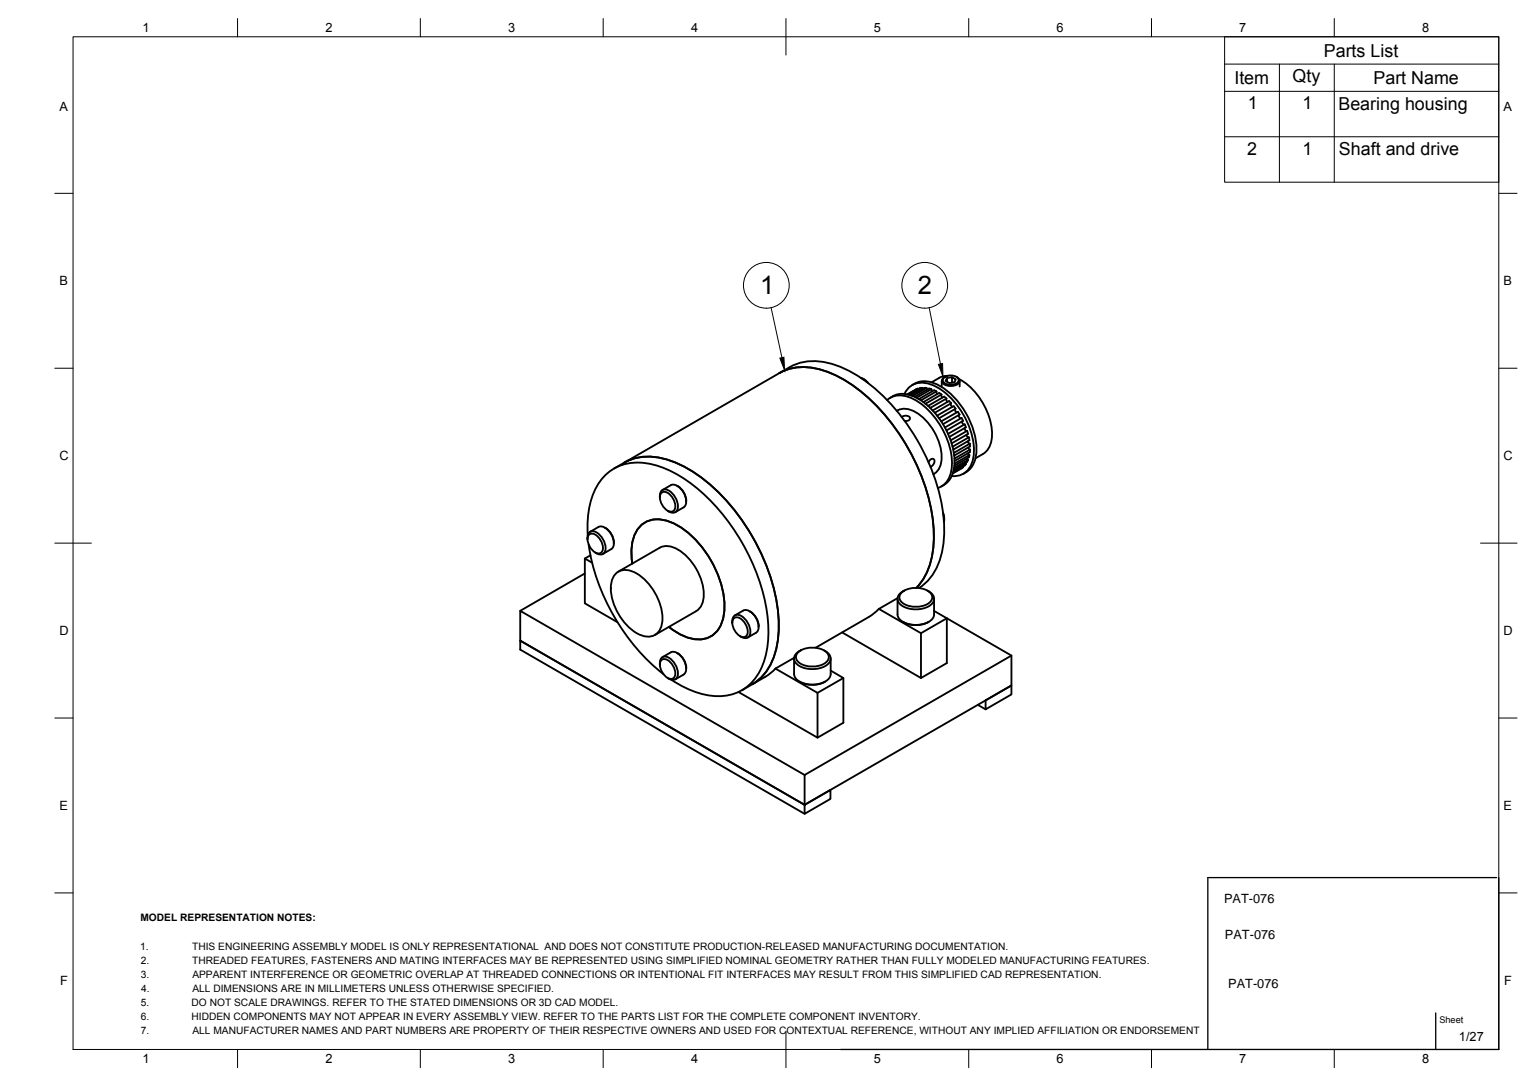
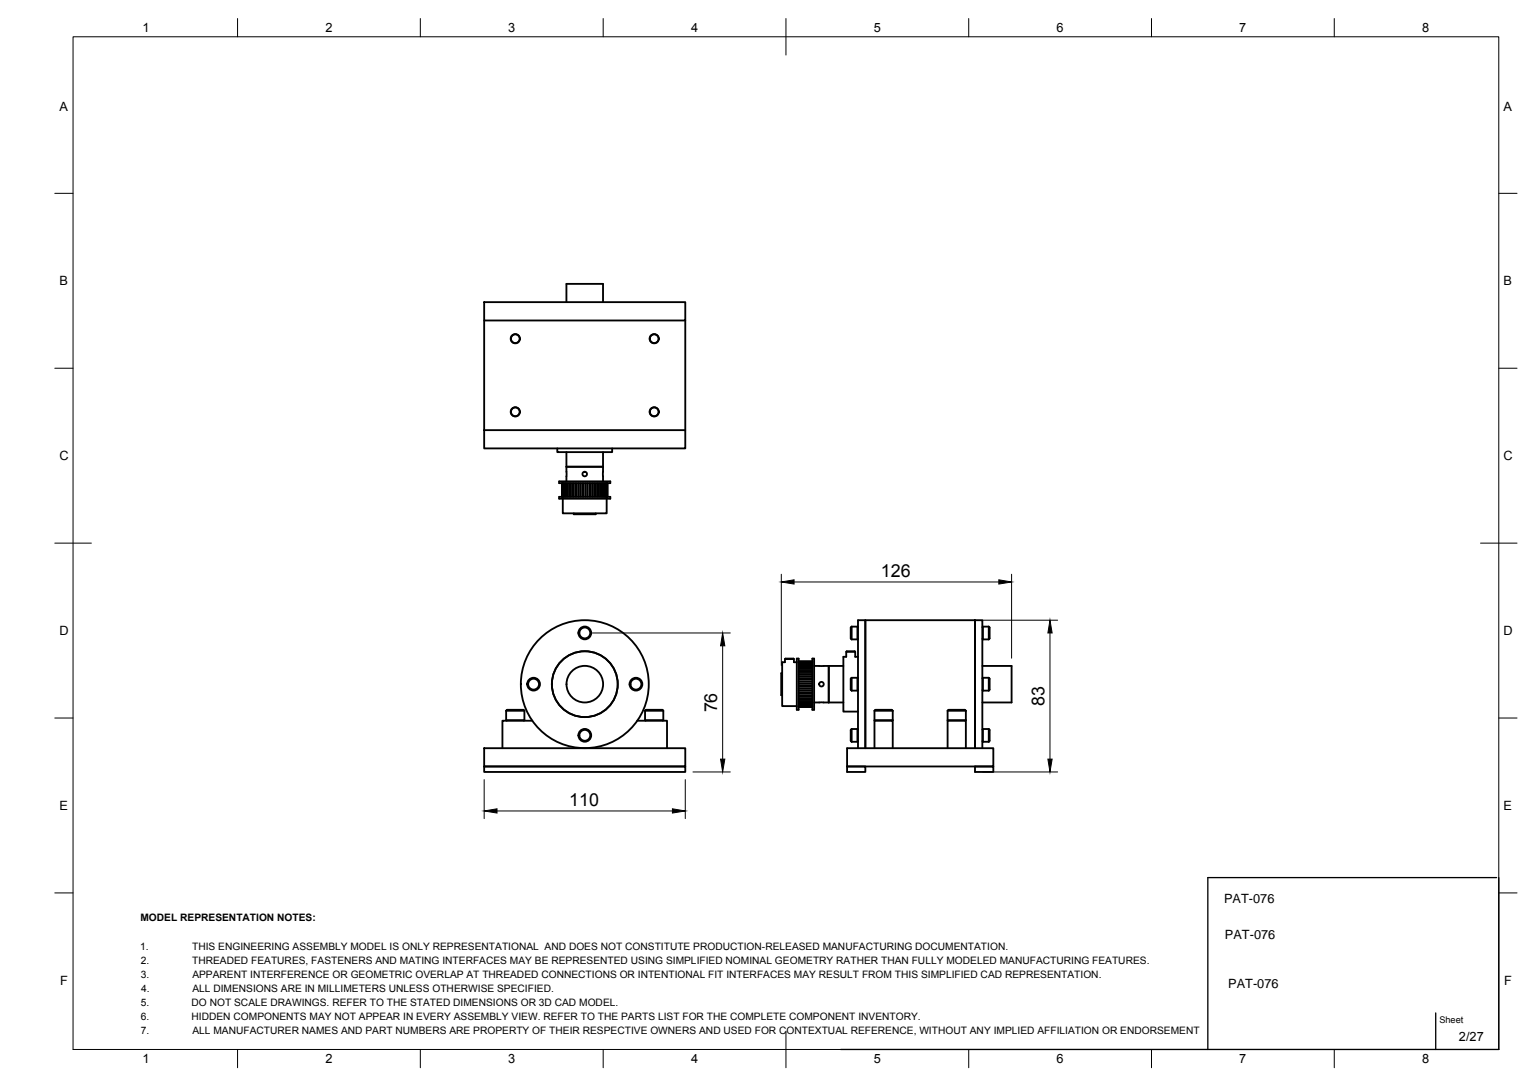
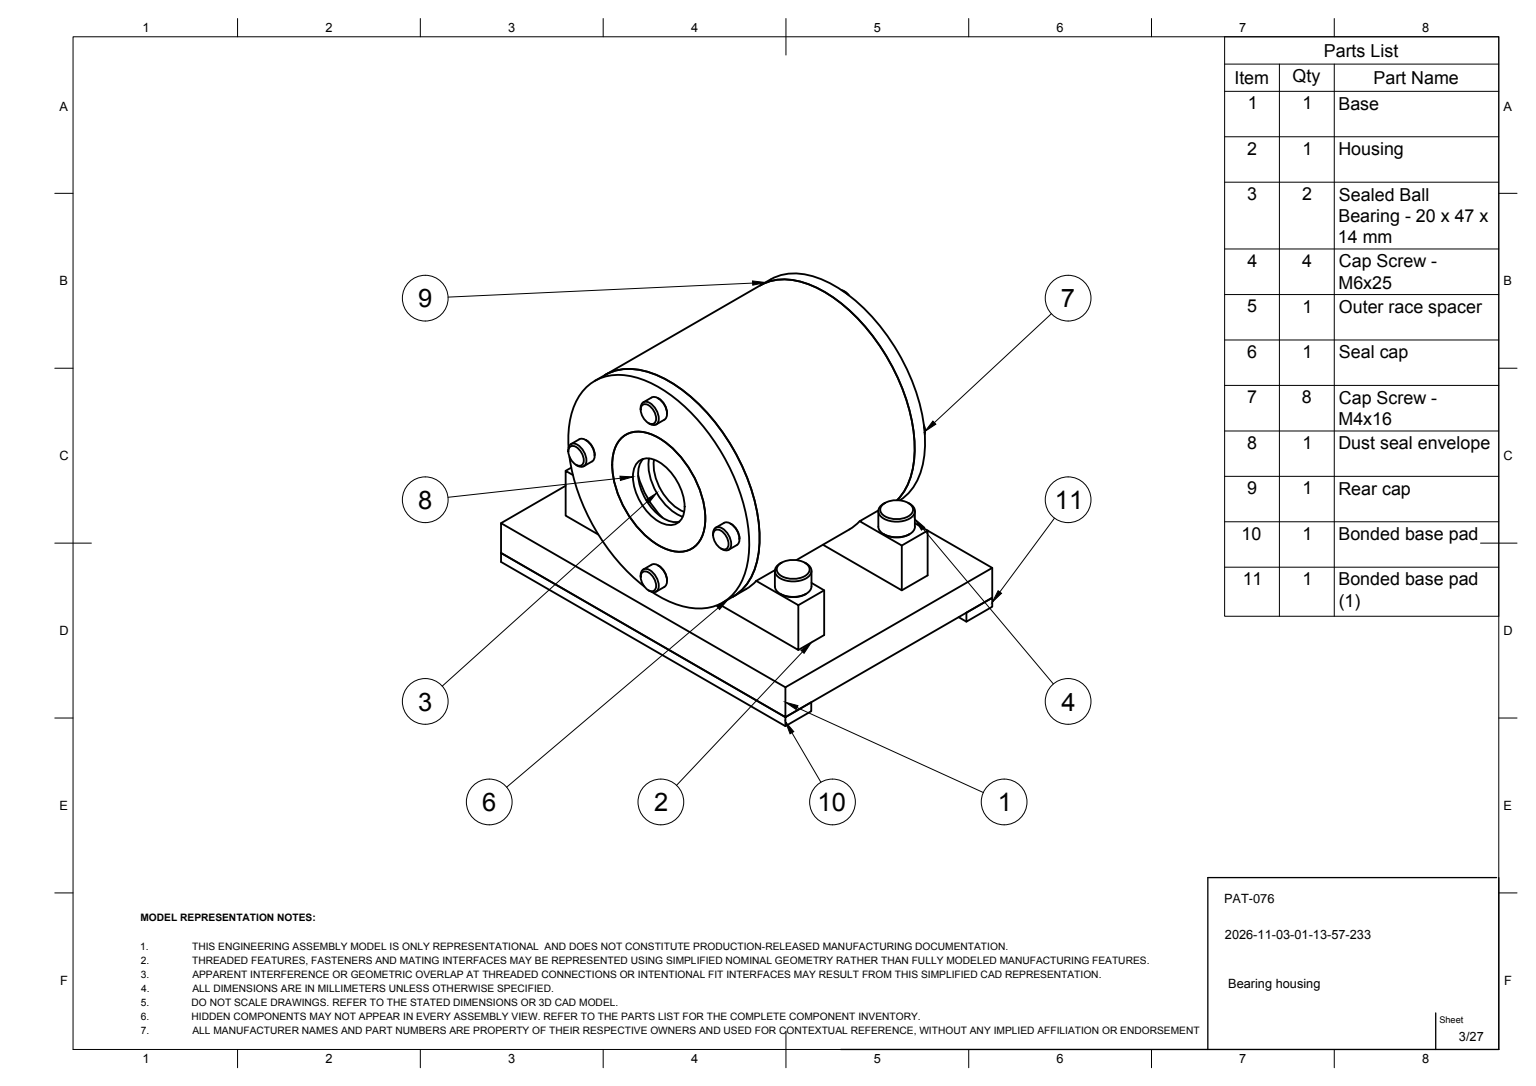
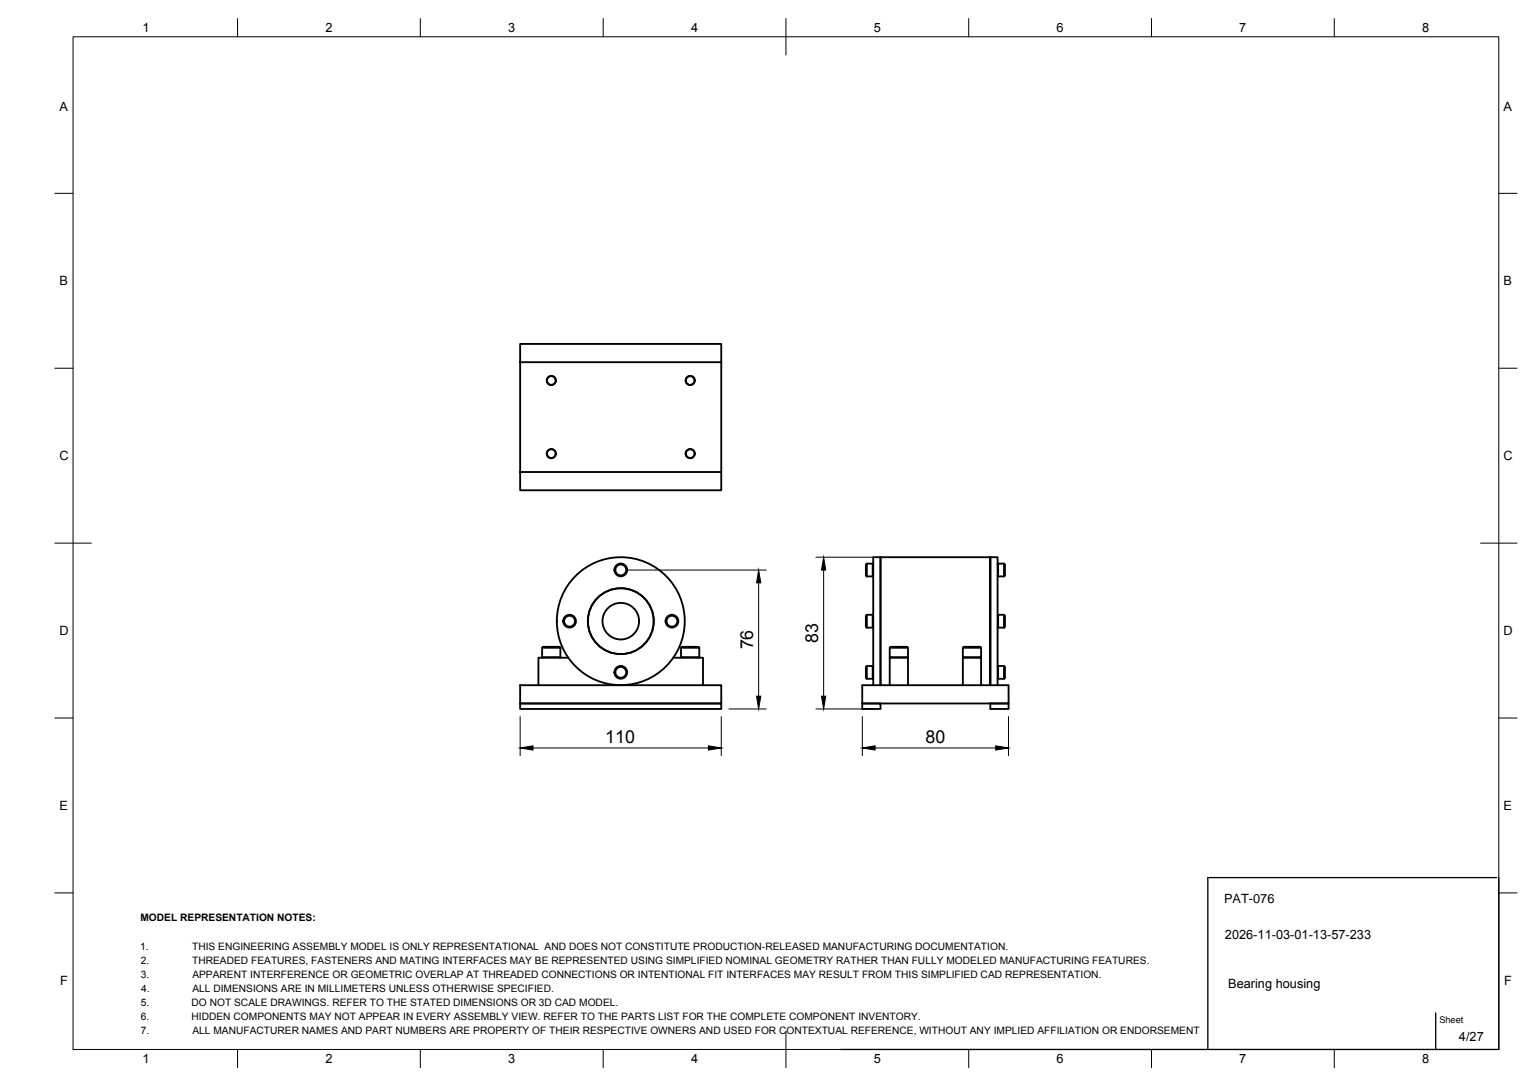
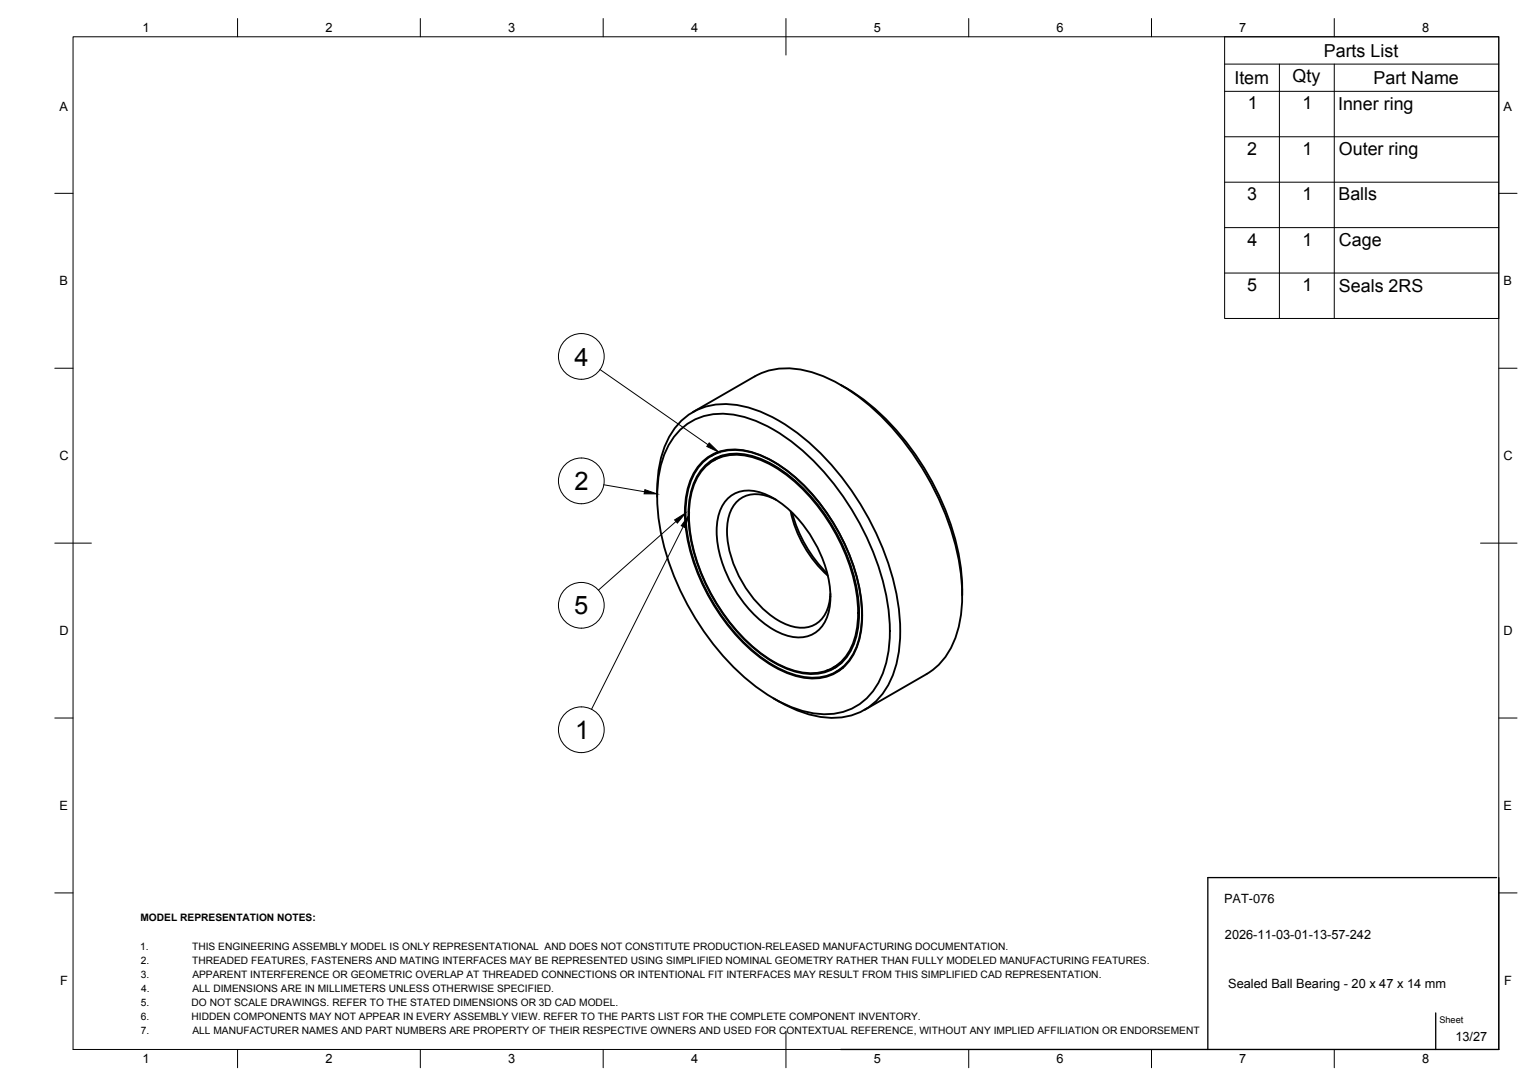
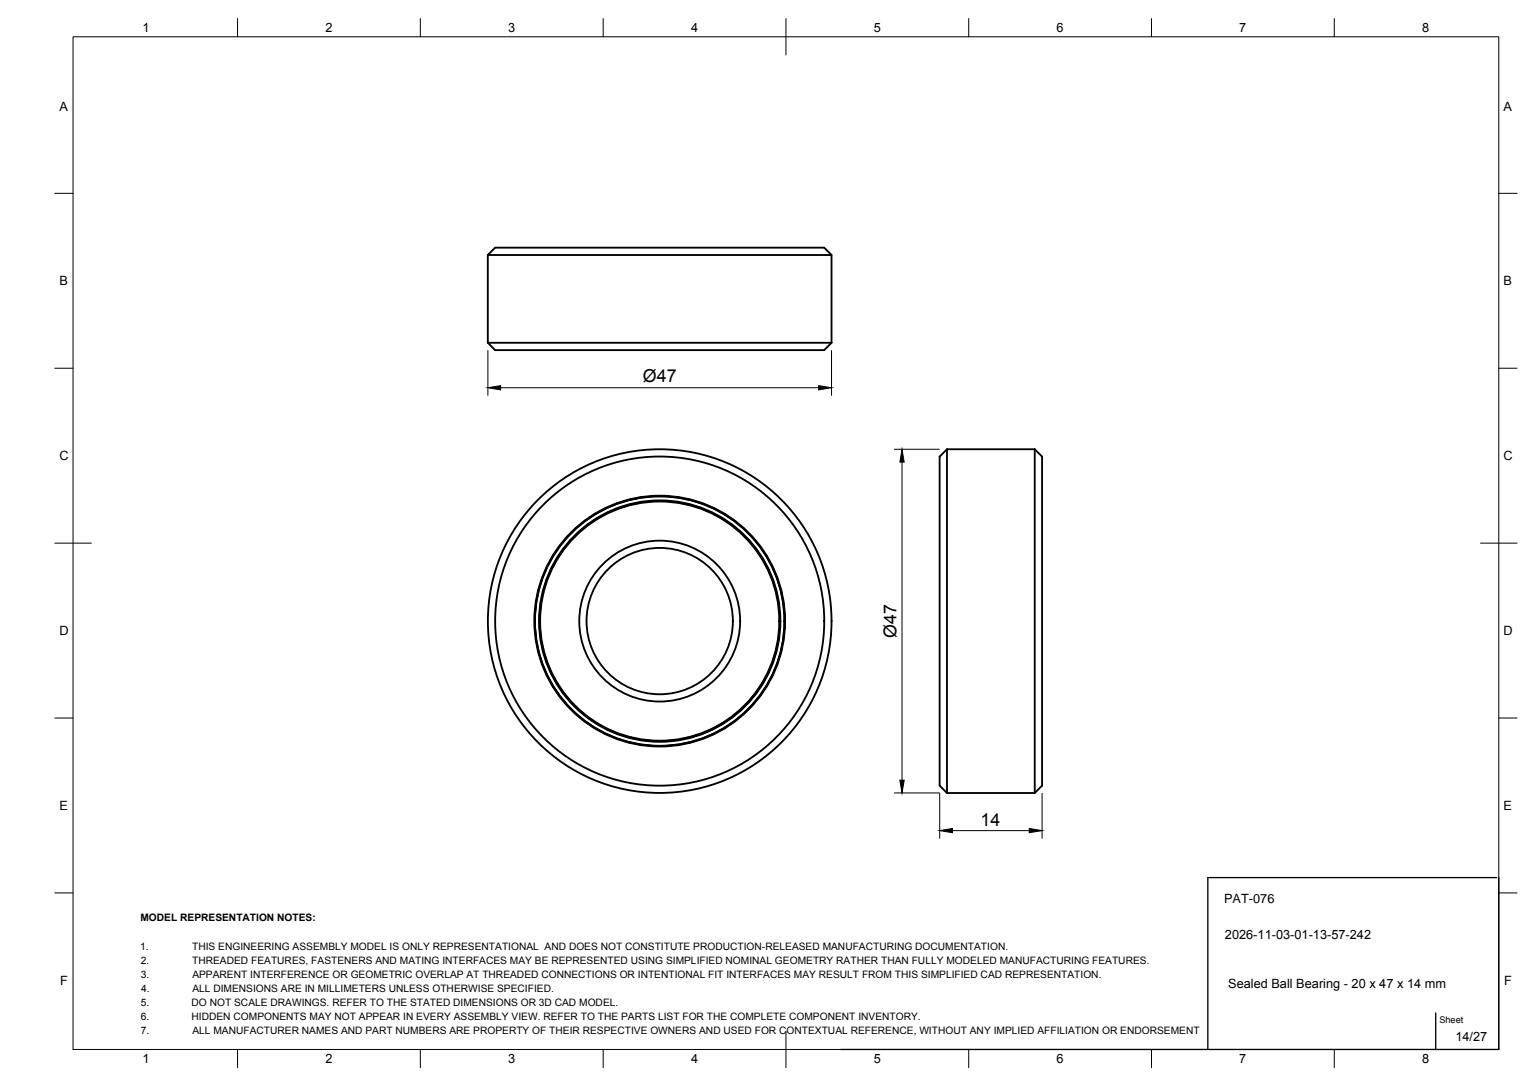
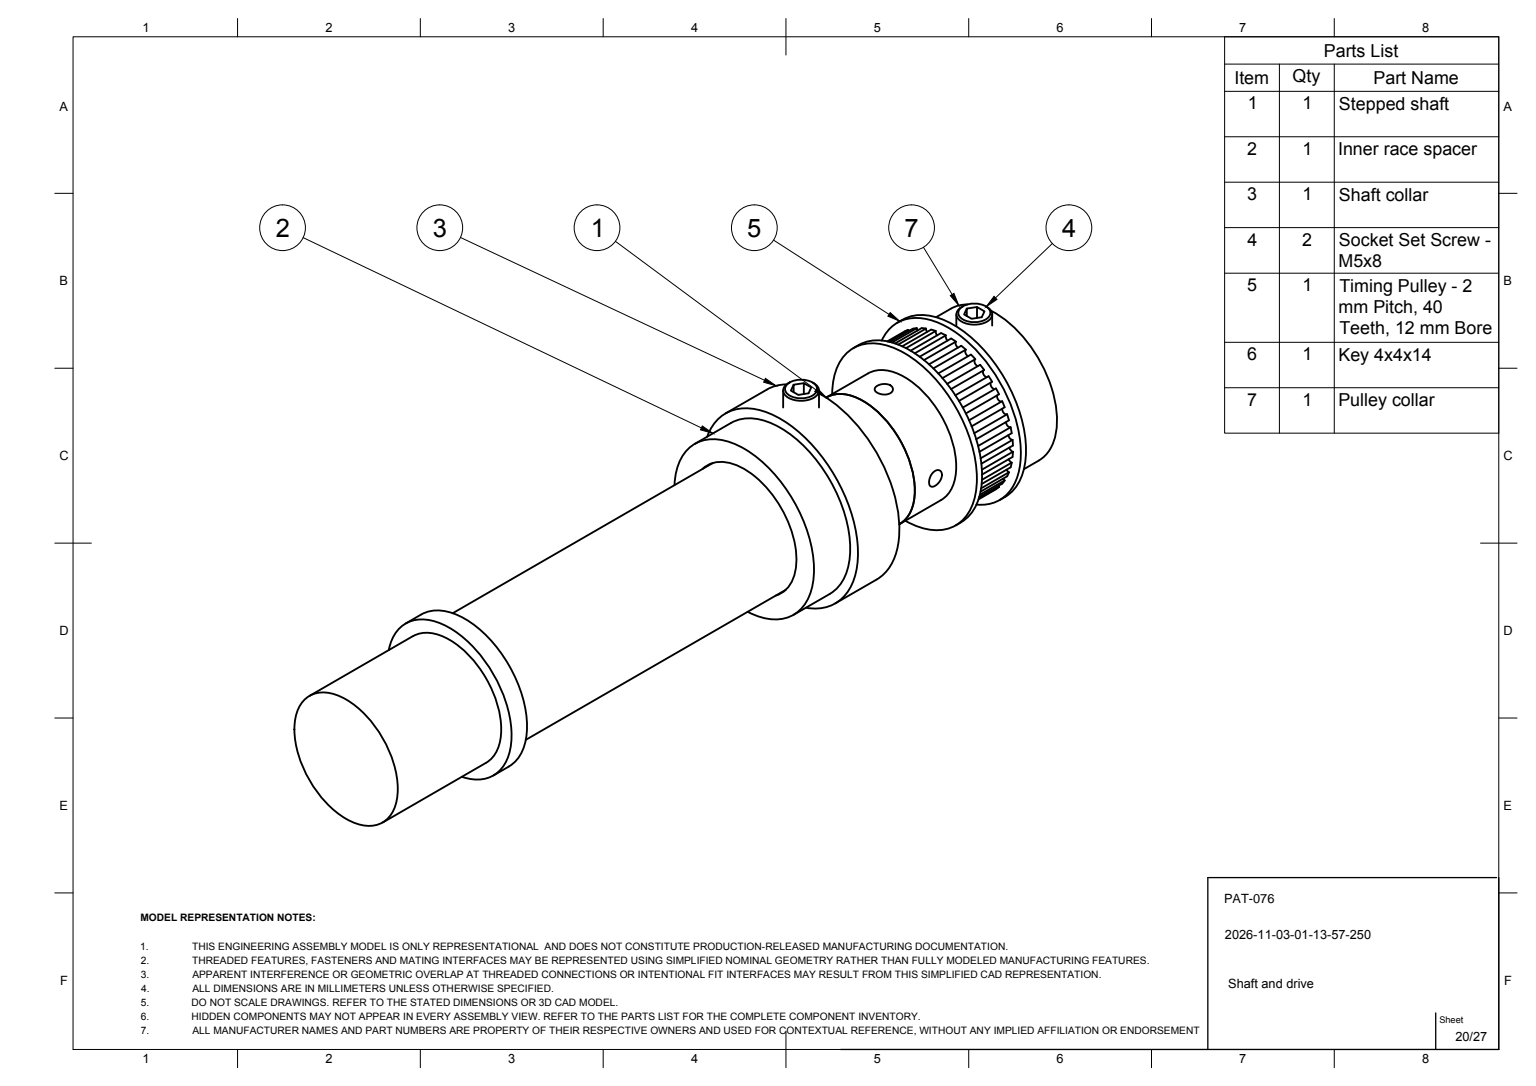
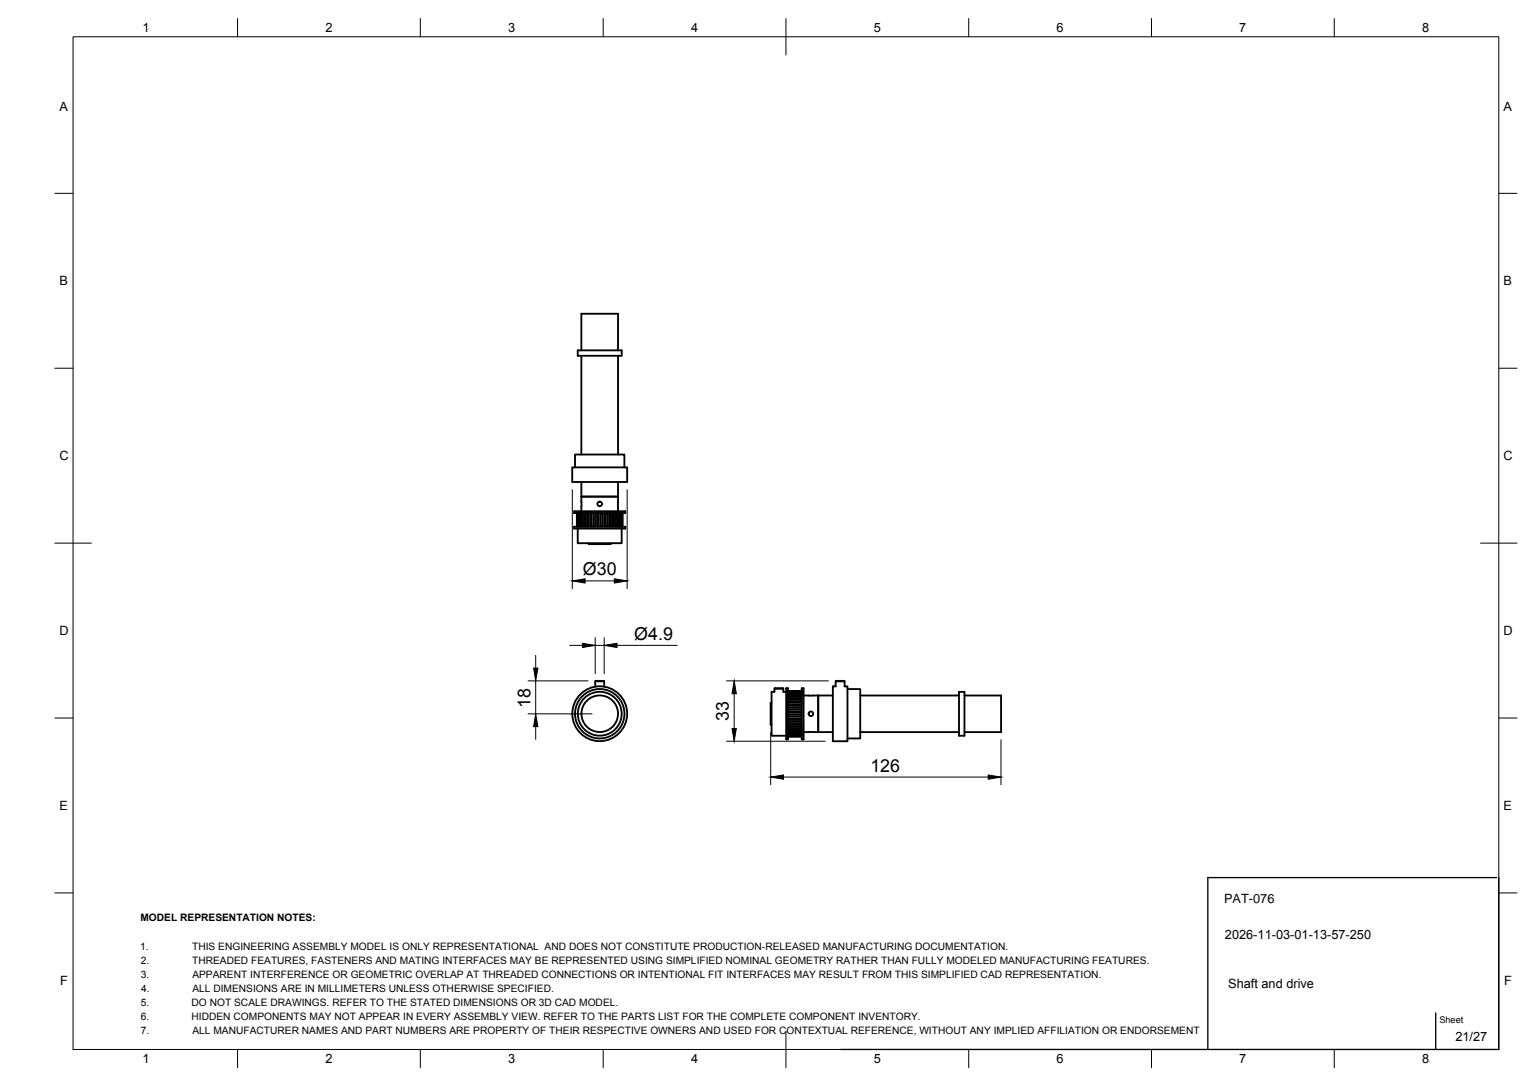
ISO-10303-21;
HEADER;
/* Generated by software containing ST-Developer
 * from STEP Tools, Inc. (www.steptools.com) 
 */

FILE_DESCRIPTION(
/* description */ ('Overhung pulley bearing cartridge'),
/* implementation_level */ '2;1');

FILE_NAME(
/* name */ 'PAT-076',
/* time_stamp */ '2026-10-28T03:22:33-07:00',
/* author */ (''),
/* organization */ (''),
/* preprocessor_version */ 'ST-DEVELOPER v20.2',
/* originating_system */ 'Autodesk Translation Framework v15.17.0.0',
/* authorisation */ '');

FILE_SCHEMA (('AUTOMOTIVE_DESIGN { 1 0 10303 214 3 1 1 }'));
ENDSEC;

DATA;
#10=MECHANICAL_DESIGN_GEOMETRIC_PRESENTATION_REPRESENTATION('',(#283,#284,
#285,#286,#287,#288,#289,#290,#291,#292,#293,#294,#295,#296,#297,#298,#299,
#300,#301,#302,#303,#304,#305,#306,#307,#308,#309,#310,#311,#312),#10963);
#11=ORIENTED_CLOSED_SHELL('',*,#5672,.F.);
#12=ORIENTED_CLOSED_SHELL('',*,#5674,.F.);
#13=BREP_WITH_VOIDS('Body1',#5671,(#11));
#14=BREP_WITH_VOIDS('Body1',#5673,(#12));
#15=ITEM_DEFINED_TRANSFORMATION($,$,#6112,#6240);
#16=ITEM_DEFINED_TRANSFORMATION($,$,#6132,#6241);
#17=ITEM_DEFINED_TRANSFORMATION($,$,#6152,#6242);
#18=ITEM_DEFINED_TRANSFORMATION($,$,#6169,#6243);
#19=ITEM_DEFINED_TRANSFORMATION($,$,#6223,#6244);
#20=ITEM_DEFINED_TRANSFORMATION($,$,#5927,#6297);
#21=ITEM_DEFINED_TRANSFORMATION($,$,#5946,#6298);
#22=ITEM_DEFINED_TRANSFORMATION($,$,#6025,#6299);
#23=ITEM_DEFINED_TRANSFORMATION($,$,#6034,#6300);
#24=ITEM_DEFINED_TRANSFORMATION($,$,#6063,#6301);
#25=ITEM_DEFINED_TRANSFORMATION($,$,#6072,#6302);
#26=ITEM_DEFINED_TRANSFORMATION($,$,#6097,#6303);
#27=ITEM_DEFINED_TRANSFORMATION($,$,#6104,#6304);
#28=ITEM_DEFINED_TRANSFORMATION($,$,#6111,#6305);
#29=ITEM_DEFINED_TRANSFORMATION($,$,#6245,#6306);
#30=ITEM_DEFINED_TRANSFORMATION($,$,#6245,#6307);
#31=ITEM_DEFINED_TRANSFORMATION($,$,#6111,#6308);
#32=ITEM_DEFINED_TRANSFORMATION($,$,#6245,#6309);
#33=ITEM_DEFINED_TRANSFORMATION($,$,#6245,#6310);
#34=ITEM_DEFINED_TRANSFORMATION($,$,#6271,#6311);
#35=ITEM_DEFINED_TRANSFORMATION($,$,#6271,#6312);
#36=ITEM_DEFINED_TRANSFORMATION($,$,#6271,#6313);
#37=ITEM_DEFINED_TRANSFORMATION($,$,#6271,#6314);
#38=ITEM_DEFINED_TRANSFORMATION($,$,#6271,#6315);
#39=ITEM_DEFINED_TRANSFORMATION($,$,#6271,#6316);
#40=ITEM_DEFINED_TRANSFORMATION($,$,#6271,#6317);
#41=ITEM_DEFINED_TRANSFORMATION($,$,#6271,#6318);
#42=ITEM_DEFINED_TRANSFORMATION($,$,#6320,#6678);
#43=ITEM_DEFINED_TRANSFORMATION($,$,#6345,#6679);
#44=ITEM_DEFINED_TRANSFORMATION($,$,#6354,#6680);
#45=ITEM_DEFINED_TRANSFORMATION($,$,#6369,#6681);
#46=ITEM_DEFINED_TRANSFORMATION($,$,#6661,#6682);
#47=ITEM_DEFINED_TRANSFORMATION($,$,#6384,#6683);
#48=ITEM_DEFINED_TRANSFORMATION($,$,#6650,#6684);
#49=ITEM_DEFINED_TRANSFORMATION($,$,#6661,#6685);
#50=ITEM_DEFINED_TRANSFORMATION($,$,#5926,#6686);
#51=ITEM_DEFINED_TRANSFORMATION($,$,#6319,#6687);
#52=(
REPRESENTATION_RELATIONSHIP($,$,#11068,#11067)
REPRESENTATION_RELATIONSHIP_WITH_TRANSFORMATION(#15)
SHAPE_REPRESENTATION_RELATIONSHIP()
);
#53=(
REPRESENTATION_RELATIONSHIP($,$,#11069,#11067)
REPRESENTATION_RELATIONSHIP_WITH_TRANSFORMATION(#16)
SHAPE_REPRESENTATION_RELATIONSHIP()
);
#54=(
REPRESENTATION_RELATIONSHIP($,$,#11070,#11067)
REPRESENTATION_RELATIONSHIP_WITH_TRANSFORMATION(#17)
SHAPE_REPRESENTATION_RELATIONSHIP()
);
#55=(
REPRESENTATION_RELATIONSHIP($,$,#11071,#11067)
REPRESENTATION_RELATIONSHIP_WITH_TRANSFORMATION(#18)
SHAPE_REPRESENTATION_RELATIONSHIP()
);
#56=(
REPRESENTATION_RELATIONSHIP($,$,#11072,#11067)
REPRESENTATION_RELATIONSHIP_WITH_TRANSFORMATION(#19)
SHAPE_REPRESENTATION_RELATIONSHIP()
);
#57=(
REPRESENTATION_RELATIONSHIP($,$,#11059,#11058)
REPRESENTATION_RELATIONSHIP_WITH_TRANSFORMATION(#20)
SHAPE_REPRESENTATION_RELATIONSHIP()
);
#58=(
REPRESENTATION_RELATIONSHIP($,$,#11060,#11058)
REPRESENTATION_RELATIONSHIP_WITH_TRANSFORMATION(#21)
SHAPE_REPRESENTATION_RELATIONSHIP()
);
#59=(
REPRESENTATION_RELATIONSHIP($,$,#11061,#11058)
REPRESENTATION_RELATIONSHIP_WITH_TRANSFORMATION(#22)
SHAPE_REPRESENTATION_RELATIONSHIP()
);
#60=(
REPRESENTATION_RELATIONSHIP($,$,#11062,#11058)
REPRESENTATION_RELATIONSHIP_WITH_TRANSFORMATION(#23)
SHAPE_REPRESENTATION_RELATIONSHIP()
);
#61=(
REPRESENTATION_RELATIONSHIP($,$,#11063,#11058)
REPRESENTATION_RELATIONSHIP_WITH_TRANSFORMATION(#24)
SHAPE_REPRESENTATION_RELATIONSHIP()
);
#62=(
REPRESENTATION_RELATIONSHIP($,$,#11064,#11058)
REPRESENTATION_RELATIONSHIP_WITH_TRANSFORMATION(#25)
SHAPE_REPRESENTATION_RELATIONSHIP()
);
#63=(
REPRESENTATION_RELATIONSHIP($,$,#11065,#11058)
REPRESENTATION_RELATIONSHIP_WITH_TRANSFORMATION(#26)
SHAPE_REPRESENTATION_RELATIONSHIP()
);
#64=(
REPRESENTATION_RELATIONSHIP($,$,#11066,#11058)
REPRESENTATION_RELATIONSHIP_WITH_TRANSFORMATION(#27)
SHAPE_REPRESENTATION_RELATIONSHIP()
);
#65=(
REPRESENTATION_RELATIONSHIP($,$,#11067,#11058)
REPRESENTATION_RELATIONSHIP_WITH_TRANSFORMATION(#28)
SHAPE_REPRESENTATION_RELATIONSHIP()
);
#66=(
REPRESENTATION_RELATIONSHIP($,$,#11073,#11058)
REPRESENTATION_RELATIONSHIP_WITH_TRANSFORMATION(#29)
SHAPE_REPRESENTATION_RELATIONSHIP()
);
#67=(
REPRESENTATION_RELATIONSHIP($,$,#11073,#11058)
REPRESENTATION_RELATIONSHIP_WITH_TRANSFORMATION(#30)
SHAPE_REPRESENTATION_RELATIONSHIP()
);
#68=(
REPRESENTATION_RELATIONSHIP($,$,#11067,#11058)
REPRESENTATION_RELATIONSHIP_WITH_TRANSFORMATION(#31)
SHAPE_REPRESENTATION_RELATIONSHIP()
);
#69=(
REPRESENTATION_RELATIONSHIP($,$,#11073,#11058)
REPRESENTATION_RELATIONSHIP_WITH_TRANSFORMATION(#32)
SHAPE_REPRESENTATION_RELATIONSHIP()
);
#70=(
REPRESENTATION_RELATIONSHIP($,$,#11073,#11058)
REPRESENTATION_RELATIONSHIP_WITH_TRANSFORMATION(#33)
SHAPE_REPRESENTATION_RELATIONSHIP()
);
#71=(
REPRESENTATION_RELATIONSHIP($,$,#11074,#11058)
REPRESENTATION_RELATIONSHIP_WITH_TRANSFORMATION(#34)
SHAPE_REPRESENTATION_RELATIONSHIP()
);
#72=(
REPRESENTATION_RELATIONSHIP($,$,#11074,#11058)
REPRESENTATION_RELATIONSHIP_WITH_TRANSFORMATION(#35)
SHAPE_REPRESENTATION_RELATIONSHIP()
);
#73=(
REPRESENTATION_RELATIONSHIP($,$,#11074,#11058)
REPRESENTATION_RELATIONSHIP_WITH_TRANSFORMATION(#36)
SHAPE_REPRESENTATION_RELATIONSHIP()
);
#74=(
REPRESENTATION_RELATIONSHIP($,$,#11074,#11058)
REPRESENTATION_RELATIONSHIP_WITH_TRANSFORMATION(#37)
SHAPE_REPRESENTATION_RELATIONSHIP()
);
#75=(
REPRESENTATION_RELATIONSHIP($,$,#11074,#11058)
REPRESENTATION_RELATIONSHIP_WITH_TRANSFORMATION(#38)
SHAPE_REPRESENTATION_RELATIONSHIP()
);
#76=(
REPRESENTATION_RELATIONSHIP($,$,#11074,#11058)
REPRESENTATION_RELATIONSHIP_WITH_TRANSFORMATION(#39)
SHAPE_REPRESENTATION_RELATIONSHIP()
);
#77=(
REPRESENTATION_RELATIONSHIP($,$,#11074,#11058)
REPRESENTATION_RELATIONSHIP_WITH_TRANSFORMATION(#40)
SHAPE_REPRESENTATION_RELATIONSHIP()
);
#78=(
REPRESENTATION_RELATIONSHIP($,$,#11074,#11058)
REPRESENTATION_RELATIONSHIP_WITH_TRANSFORMATION(#41)
SHAPE_REPRESENTATION_RELATIONSHIP()
);
#79=(
REPRESENTATION_RELATIONSHIP($,$,#11076,#11075)
REPRESENTATION_RELATIONSHIP_WITH_TRANSFORMATION(#42)
SHAPE_REPRESENTATION_RELATIONSHIP()
);
#80=(
REPRESENTATION_RELATIONSHIP($,$,#11077,#11075)
REPRESENTATION_RELATIONSHIP_WITH_TRANSFORMATION(#43)
SHAPE_REPRESENTATION_RELATIONSHIP()
);
#81=(
REPRESENTATION_RELATIONSHIP($,$,#11078,#11075)
REPRESENTATION_RELATIONSHIP_WITH_TRANSFORMATION(#44)
SHAPE_REPRESENTATION_RELATIONSHIP()
);
#82=(
REPRESENTATION_RELATIONSHIP($,$,#11079,#11075)
REPRESENTATION_RELATIONSHIP_WITH_TRANSFORMATION(#45)
SHAPE_REPRESENTATION_RELATIONSHIP()
);
#83=(
REPRESENTATION_RELATIONSHIP($,$,#11082,#11075)
REPRESENTATION_RELATIONSHIP_WITH_TRANSFORMATION(#46)
SHAPE_REPRESENTATION_RELATIONSHIP()
);
#84=(
REPRESENTATION_RELATIONSHIP($,$,#11080,#11075)
REPRESENTATION_RELATIONSHIP_WITH_TRANSFORMATION(#47)
SHAPE_REPRESENTATION_RELATIONSHIP()
);
#85=(
REPRESENTATION_RELATIONSHIP($,$,#11081,#11075)
REPRESENTATION_RELATIONSHIP_WITH_TRANSFORMATION(#48)
SHAPE_REPRESENTATION_RELATIONSHIP()
);
#86=(
REPRESENTATION_RELATIONSHIP($,$,#11082,#11075)
REPRESENTATION_RELATIONSHIP_WITH_TRANSFORMATION(#49)
SHAPE_REPRESENTATION_RELATIONSHIP()
);
#87=(
REPRESENTATION_RELATIONSHIP($,$,#11058,#11057)
REPRESENTATION_RELATIONSHIP_WITH_TRANSFORMATION(#50)
SHAPE_REPRESENTATION_RELATIONSHIP()
);
#88=(
REPRESENTATION_RELATIONSHIP($,$,#11075,#11057)
REPRESENTATION_RELATIONSHIP_WITH_TRANSFORMATION(#51)
SHAPE_REPRESENTATION_RELATIONSHIP()
);
#89=CONTEXT_DEPENDENT_SHAPE_REPRESENTATION(#52,#11010);
#90=CONTEXT_DEPENDENT_SHAPE_REPRESENTATION(#53,#11011);
#91=CONTEXT_DEPENDENT_SHAPE_REPRESENTATION(#54,#11012);
#92=CONTEXT_DEPENDENT_SHAPE_REPRESENTATION(#55,#11013);
#93=CONTEXT_DEPENDENT_SHAPE_REPRESENTATION(#56,#11014);
#94=CONTEXT_DEPENDENT_SHAPE_REPRESENTATION(#57,#11017);
#95=CONTEXT_DEPENDENT_SHAPE_REPRESENTATION(#58,#11018);
#96=CONTEXT_DEPENDENT_SHAPE_REPRESENTATION(#59,#11019);
#97=CONTEXT_DEPENDENT_SHAPE_REPRESENTATION(#60,#11020);
#98=CONTEXT_DEPENDENT_SHAPE_REPRESENTATION(#61,#11021);
#99=CONTEXT_DEPENDENT_SHAPE_REPRESENTATION(#62,#11022);
#100=CONTEXT_DEPENDENT_SHAPE_REPRESENTATION(#63,#11023);
#101=CONTEXT_DEPENDENT_SHAPE_REPRESENTATION(#64,#11024);
#102=CONTEXT_DEPENDENT_SHAPE_REPRESENTATION(#65,#11025);
#103=CONTEXT_DEPENDENT_SHAPE_REPRESENTATION(#66,#11026);
#104=CONTEXT_DEPENDENT_SHAPE_REPRESENTATION(#67,#11027);
#105=CONTEXT_DEPENDENT_SHAPE_REPRESENTATION(#68,#11028);
#106=CONTEXT_DEPENDENT_SHAPE_REPRESENTATION(#69,#11029);
#107=CONTEXT_DEPENDENT_SHAPE_REPRESENTATION(#70,#11030);
#108=CONTEXT_DEPENDENT_SHAPE_REPRESENTATION(#71,#11031);
#109=CONTEXT_DEPENDENT_SHAPE_REPRESENTATION(#72,#11032);
#110=CONTEXT_DEPENDENT_SHAPE_REPRESENTATION(#73,#11033);
#111=CONTEXT_DEPENDENT_SHAPE_REPRESENTATION(#74,#11034);
#112=CONTEXT_DEPENDENT_SHAPE_REPRESENTATION(#75,#11035);
#113=CONTEXT_DEPENDENT_SHAPE_REPRESENTATION(#76,#11036);
#114=CONTEXT_DEPENDENT_SHAPE_REPRESENTATION(#77,#11037);
#115=CONTEXT_DEPENDENT_SHAPE_REPRESENTATION(#78,#11038);
#116=CONTEXT_DEPENDENT_SHAPE_REPRESENTATION(#79,#11047);
#117=CONTEXT_DEPENDENT_SHAPE_REPRESENTATION(#80,#11048);
#118=CONTEXT_DEPENDENT_SHAPE_REPRESENTATION(#81,#11049);
#119=CONTEXT_DEPENDENT_SHAPE_REPRESENTATION(#82,#11050);
#120=CONTEXT_DEPENDENT_SHAPE_REPRESENTATION(#83,#11051);
#121=CONTEXT_DEPENDENT_SHAPE_REPRESENTATION(#84,#11052);
#122=CONTEXT_DEPENDENT_SHAPE_REPRESENTATION(#85,#11053);
#123=CONTEXT_DEPENDENT_SHAPE_REPRESENTATION(#86,#11054);
#124=CONTEXT_DEPENDENT_SHAPE_REPRESENTATION(#87,#11055);
#125=CONTEXT_DEPENDENT_SHAPE_REPRESENTATION(#88,#11056);
#126=NEXT_ASSEMBLY_USAGE_OCCURRENCE('Inner ring:1','Inner ring:1',
'Inner ring:1',#11094,#11095,'Inner ring:1');
#127=NEXT_ASSEMBLY_USAGE_OCCURRENCE('Outer ring:1','Outer ring:1',
'Outer ring:1',#11094,#11096,'Outer ring:1');
#128=NEXT_ASSEMBLY_USAGE_OCCURRENCE('Balls:1','Balls:1','Balls:1',#11094,
#11097,'Balls:1');
#129=NEXT_ASSEMBLY_USAGE_OCCURRENCE('Cage:1','Cage:1','Cage:1',#11094,#11098,
'Cage:1');
#130=NEXT_ASSEMBLY_USAGE_OCCURRENCE('Seals 2RS:1','Seals 2RS:1',
'Seals 2RS:1',#11094,#11099,'Seals 2RS:1');
#131=NEXT_ASSEMBLY_USAGE_OCCURRENCE('Base:1','Base:1','Base:1',#11085,#11086,
'Base:1');
#132=NEXT_ASSEMBLY_USAGE_OCCURRENCE('Housing:1','Housing:1','Housing:1',
#11085,#11087,'Housing:1');
#133=NEXT_ASSEMBLY_USAGE_OCCURRENCE('Outer race spacer:1',
'Outer race spacer:1','Outer race spacer:1',#11085,#11088,
'Outer race spacer:1');
#134=NEXT_ASSEMBLY_USAGE_OCCURRENCE('Seal cap:1','Seal cap:1',
'Seal cap:1',#11085,#11089,'Seal cap:1');
#135=NEXT_ASSEMBLY_USAGE_OCCURRENCE('Dust seal envelope:1',
'Dust seal envelope:1','Dust seal envelope:1',#11085,#11090,
'Dust seal envelope:1');
#136=NEXT_ASSEMBLY_USAGE_OCCURRENCE('Rear cap:1','Rear cap:1',
'Rear cap:1',#11085,#11091,'Rear cap:1');
#137=NEXT_ASSEMBLY_USAGE_OCCURRENCE('Bonded base pad:1',
'Bonded base pad:1','Bonded base pad:1',#11085,#11092,
'Bonded base pad:1');
#138=NEXT_ASSEMBLY_USAGE_OCCURRENCE('Bonded base pad (1):1',
'Bonded base pad (1):1','Bonded base pad (1):1',#11085,#11093,
'Bonded base pad (1):1');
#139=NEXT_ASSEMBLY_USAGE_OCCURRENCE(
'Sealed Ball Bearing - 20 x 47 x 14 mm:2',
'Sealed Ball Bearing - 20 x 47 x 14 mm:2',
'Sealed Ball Bearing - 20 x 47 x 14 mm:2',#11085,#11094,
'Sealed Ball Bearing - 20 x 47 x 14 mm:2');
#140=NEXT_ASSEMBLY_USAGE_OCCURRENCE('Cap Screw - M6x25:2',
'Cap Screw - M6x25:2','Cap Screw - M6x25:2',#11085,#11100,
'Cap Screw - M6x25:2');
#141=NEXT_ASSEMBLY_USAGE_OCCURRENCE('Cap Screw - M6x25:3',
'Cap Screw - M6x25:3','Cap Screw - M6x25:3',#11085,#11100,
'Cap Screw - M6x25:3');
#142=NEXT_ASSEMBLY_USAGE_OCCURRENCE(
'Sealed Ball Bearing - 20 x 47 x 14 mm:3',
'Sealed Ball Bearing - 20 x 47 x 14 mm:3',
'Sealed Ball Bearing - 20 x 47 x 14 mm:3',#11085,#11094,
'Sealed Ball Bearing - 20 x 47 x 14 mm:3');
#143=NEXT_ASSEMBLY_USAGE_OCCURRENCE('Cap Screw - M6x25:4',
'Cap Screw - M6x25:4','Cap Screw - M6x25:4',#11085,#11100,
'Cap Screw - M6x25:4');
#144=NEXT_ASSEMBLY_USAGE_OCCURRENCE('Cap Screw - M6x25:5',
'Cap Screw - M6x25:5','Cap Screw - M6x25:5',#11085,#11100,
'Cap Screw - M6x25:5');
#145=NEXT_ASSEMBLY_USAGE_OCCURRENCE('Cap Screw - M4x16:2',
'Cap Screw - M4x16:2','Cap Screw - M4x16:2',#11085,#11101,
'Cap Screw - M4x16:2');
#146=NEXT_ASSEMBLY_USAGE_OCCURRENCE('Cap Screw - M4x16:3',
'Cap Screw - M4x16:3','Cap Screw - M4x16:3',#11085,#11101,
'Cap Screw - M4x16:3');
#147=NEXT_ASSEMBLY_USAGE_OCCURRENCE('Cap Screw - M4x16:4',
'Cap Screw - M4x16:4','Cap Screw - M4x16:4',#11085,#11101,
'Cap Screw - M4x16:4');
#148=NEXT_ASSEMBLY_USAGE_OCCURRENCE('Cap Screw - M4x16:5',
'Cap Screw - M4x16:5','Cap Screw - M4x16:5',#11085,#11101,
'Cap Screw - M4x16:5');
#149=NEXT_ASSEMBLY_USAGE_OCCURRENCE('Cap Screw - M4x16:6',
'Cap Screw - M4x16:6','Cap Screw - M4x16:6',#11085,#11101,
'Cap Screw - M4x16:6');
#150=NEXT_ASSEMBLY_USAGE_OCCURRENCE('Cap Screw - M4x16:7',
'Cap Screw - M4x16:7','Cap Screw - M4x16:7',#11085,#11101,
'Cap Screw - M4x16:7');
#151=NEXT_ASSEMBLY_USAGE_OCCURRENCE('Cap Screw - M4x16:8',
'Cap Screw - M4x16:8','Cap Screw - M4x16:8',#11085,#11101,
'Cap Screw - M4x16:8');
#152=NEXT_ASSEMBLY_USAGE_OCCURRENCE('Cap Screw - M4x16:9',
'Cap Screw - M4x16:9','Cap Screw - M4x16:9',#11085,#11101,
'Cap Screw - M4x16:9');
#153=NEXT_ASSEMBLY_USAGE_OCCURRENCE('Stepped shaft:1','Stepped shaft:1',
'Stepped shaft:1',#11102,#11103,'Stepped shaft:1');
#154=NEXT_ASSEMBLY_USAGE_OCCURRENCE('Inner race spacer:1',
'Inner race spacer:1','Inner race spacer:1',#11102,#11104,
'Inner race spacer:1');
#155=NEXT_ASSEMBLY_USAGE_OCCURRENCE('Shaft collar:1','Shaft collar:1',
'Shaft collar:1',#11102,#11105,'Shaft collar:1');
#156=NEXT_ASSEMBLY_USAGE_OCCURRENCE('Pulley collar:1','Pulley collar:1',
'Pulley collar:1',#11102,#11106,'Pulley collar:1');
#157=NEXT_ASSEMBLY_USAGE_OCCURRENCE('Socket Set Screw - M5x8:2',
'Socket Set Screw - M5x8:2','Socket Set Screw - M5x8:2',#11102,#11109,
'Socket Set Screw - M5x8:2');
#158=NEXT_ASSEMBLY_USAGE_OCCURRENCE(
'Timing Pulley - 2 mm Pitch, 40 Teeth, 12 mm Bore:2',
'Timing Pulley - 2 mm Pitch, 40 Teeth, 12 mm Bore:2',
'Timing Pulley - 2 mm Pitch, 40 Teeth, 12 mm Bore:2',#11102,#11107,
'Timing Pulley - 2 mm Pitch, 40 Teeth, 12 mm Bore:2');
#159=NEXT_ASSEMBLY_USAGE_OCCURRENCE('Key 4x4x14:2','Key 4x4x14:2',
'Key 4x4x14:2',#11102,#11108,'Key 4x4x14:2');
#160=NEXT_ASSEMBLY_USAGE_OCCURRENCE('Socket Set Screw - M5x8:3',
'Socket Set Screw - M5x8:3','Socket Set Screw - M5x8:3',#11102,#11109,
'Socket Set Screw - M5x8:3');
#161=NEXT_ASSEMBLY_USAGE_OCCURRENCE('Bearing housing:1',
'Bearing housing:1','Bearing housing:1',#11084,#11085,
'Bearing housing:1');
#162=NEXT_ASSEMBLY_USAGE_OCCURRENCE('Shaft and drive:1',
'Shaft and drive:1','Shaft and drive:1',#11084,#11102,
'Shaft and drive:1');
#163=B_SPLINE_CURVE_WITH_KNOTS('',3,(#9085,#9086,#9087,#9088,#9089,#9090,
#9091,#9092,#9093,#9094,#9095,#9096,#9097,#9098,#9099,#9100,#9101,#9102,
#9103,#9104,#9105,#9106),.UNSPECIFIED.,.F.,.F.,(4,2,2,2,2,2,2,2,2,2,4),
(0.0789094028588958,0.210573405340968,0.315860108011452,0.421146810681936,
0.522142632548711,0.623138454415485,0.72413427628226,0.825130098149035,
0.930416800819519,1.03570350349,1.16736750597208),.UNSPECIFIED.);
#164=B_SPLINE_CURVE_WITH_KNOTS('',3,(#9110,#9111,#9112,#9113,#9114,#9115,
#9116,#9117,#9118,#9119,#9120,#9121,#9122,#9123,#9124,#9125,#9126,#9127,
#9128,#9129,#9130,#9131),.UNSPECIFIED.,.F.,.F.,(4,2,2,2,2,2,2,2,2,2,4),
(0.0774793363974613,0.142088896491891,0.284177792983782,0.411119756996526,
0.514392970548519,0.617666184100513,0.720939397652506,0.8242126112045,0.951154575217244,
1.09324347170913,1.15785303180356),.UNSPECIFIED.);
#165=B_SPLINE_CURVE_WITH_KNOTS('',3,(#9137,#9138,#9139,#9140,#9141,#9142,
#9143,#9144,#9145,#9146,#9147,#9148,#9149,#9150,#9151,#9152,#9153,#9154,
#9155,#9156,#9157,#9158),.UNSPECIFIED.,.F.,.F.,(4,2,2,2,2,2,2,2,2,2,4),
(0.0774793363974613,0.142088896491891,0.284177792983782,0.411119756996525,
0.514392970548519,0.617666184100513,0.720939397652506,0.8242126112045,0.951154575217243,
1.09324347170913,1.15785303180356),.UNSPECIFIED.);
#166=B_SPLINE_CURVE_WITH_KNOTS('',3,(#9162,#9163,#9164,#9165,#9166,#9167,
#9168,#9169,#9170,#9171,#9172,#9173,#9174,#9175,#9176,#9177,#9178,#9179,
#9180,#9181,#9182,#9183),.UNSPECIFIED.,.F.,.F.,(4,2,2,2,2,2,2,2,2,2,4),
(0.0774793363974614,0.142088896491891,0.284177792983781,0.411119756996525,
0.514392970548519,0.617666184100512,0.720939397652506,0.824212611204499,
0.951154575217243,1.09324347170913,1.15785303180356),.UNSPECIFIED.);
#167=B_SPLINE_CURVE_WITH_KNOTS('',3,(#9187,#9188,#9189,#9190,#9191,#9192,
#9193,#9194,#9195,#9196,#9197,#9198),.UNSPECIFIED.,.F.,.F.,(4,2,2,2,2,4),
(0.0774793363974613,0.142088896491891,0.284177792983781,0.411119756996525,
0.514392970548519,0.617666184100512),.UNSPECIFIED.);
#168=B_SPLINE_CURVE_WITH_KNOTS('',3,(#9203,#9204,#9205,#9206,#9207,#9208,
#9209,#9210,#9211,#9212,#9213,#9214),.UNSPECIFIED.,.F.,.F.,(4,2,2,2,2,4),
(0.617666184100512,0.720939397652506,0.824212611204499,0.951154575217243,
1.09324347170913,1.15785303180356),.UNSPECIFIED.);
#169=B_SPLINE_CURVE_WITH_KNOTS('',3,(#9218,#9219,#9220,#9221,#9222,#9223,
#9224,#9225,#9226,#9227,#9228,#9229,#9230,#9231,#9232,#9233,#9234,#9235,
#9236,#9237,#9238,#9239),.UNSPECIFIED.,.F.,.F.,(4,2,2,2,2,2,2,2,2,2,4),
(0.0774793363974613,0.142088896491891,0.284177792983782,0.411119756996526,
0.514392970548519,0.617666184100513,0.720939397652507,0.8242126112045,0.951154575217245,
1.09324347170914,1.15785303180356),.UNSPECIFIED.);
#170=B_SPLINE_CURVE_WITH_KNOTS('',3,(#9243,#9244,#9245,#9246,#9247,#9248,
#9249,#9250,#9251,#9252,#9253,#9254,#9255,#9256,#9257,#9258,#9259,#9260,
#9261,#9262,#9263,#9264),.UNSPECIFIED.,.F.,.F.,(4,2,2,2,2,2,2,2,2,2,4),
(0.0774793363974613,0.142088896491891,0.284177792983782,0.411119756996526,
0.514392970548519,0.617666184100513,0.720939397652506,0.824212611204499,
0.951154575217243,1.09324347170913,1.15785303180356),.UNSPECIFIED.);
#171=B_SPLINE_CURVE_WITH_KNOTS('',3,(#9268,#9269,#9270,#9271,#9272,#9273,
#9274,#9275,#9276,#9277,#9278,#9279,#9280,#9281,#9282,#9283,#9284,#9285,
#9286,#9287,#9288,#9289),.UNSPECIFIED.,.F.,.F.,(4,2,2,2,2,2,2,2,2,2,4),
(0.0774793363974613,0.142088896491891,0.284177792983782,0.411119756996526,
0.514392970548519,0.617666184100513,0.720939397652506,0.8242126112045,0.951154575217244,
1.09324347170913,1.15785303180356),.UNSPECIFIED.);
#172=B_SPLINE_CURVE_WITH_KNOTS('',3,(#9293,#9294,#9295,#9296,#9297,#9298,
#9299,#9300,#9301,#9302,#9303,#9304,#9305,#9306,#9307,#9308,#9309,#9310,
#9311,#9312,#9313,#9314),.UNSPECIFIED.,.F.,.F.,(4,2,2,2,2,2,2,2,2,2,4),
(0.0774793363974613,0.142088896491891,0.284177792983782,0.411119756996526,
0.514392970548519,0.617666184100513,0.720939397652506,0.8242126112045,0.951154575217243,
1.09324347170913,1.15785303180356),.UNSPECIFIED.);
#173=B_SPLINE_CURVE_WITH_KNOTS('',3,(#9322,#9323,#9324,#9325,#9326,#9327,
#9328,#9329,#9330,#9331,#9332,#9333,#9334,#9335,#9336,#9337,#9338,#9339,
#9340,#9341,#9342,#9343),.UNSPECIFIED.,.F.,.F.,(4,2,2,2,2,2,2,2,2,2,4),
(0.0789094028588958,0.210573405340968,0.315860108011452,0.421146810681936,
0.522142632548711,0.623138454415485,0.72413427628226,0.825130098149035,
0.930416800819519,1.03570350349,1.16736750597208),.UNSPECIFIED.);
#174=B_SPLINE_CURVE_WITH_KNOTS('',3,(#9351,#9352,#9353,#9354,#9355,#9356,
#9357,#9358,#9359,#9360,#9361,#9362,#9363,#9364,#9365,#9366,#9367,#9368,
#9369,#9370,#9371,#9372),.UNSPECIFIED.,.F.,.F.,(4,2,2,2,2,2,2,2,2,2,4),
(0.0789094028588958,0.210573405340969,0.315860108011453,0.421146810681937,
0.522142632548712,0.623138454415486,0.724134276282261,0.825130098149035,
0.930416800819519,1.03570350349,1.16736750597208),.UNSPECIFIED.);
#175=B_SPLINE_CURVE_WITH_KNOTS('',3,(#9381,#9382,#9383,#9384,#9385,#9386,
#9387,#9388,#9389,#9390,#9391,#9392),.UNSPECIFIED.,.F.,.F.,(4,2,2,2,2,4),
(0.0789094028588958,0.210573405340968,0.315860108011452,0.421146810681937,
0.522142632548711,0.623138454415486),.UNSPECIFIED.);
#176=B_SPLINE_CURVE_WITH_KNOTS('',3,(#9394,#9395,#9396,#9397,#9398,#9399,
#9400,#9401,#9402,#9403,#9404,#9405),.UNSPECIFIED.,.F.,.F.,(4,2,2,2,2,4),
(0.623138454415486,0.72413427628226,0.825130098149035,0.930416800819519,
1.03570350349,1.16736750597208),.UNSPECIFIED.);
#177=B_SPLINE_CURVE_WITH_KNOTS('',3,(#9412,#9413,#9414,#9415,#9416,#9417,
#9418,#9419,#9420,#9421,#9422,#9423,#9424,#9425,#9426,#9427,#9428,#9429,
#9430,#9431,#9432,#9433),.UNSPECIFIED.,.F.,.F.,(4,2,2,2,2,2,2,2,2,2,4),
(0.0789094028588958,0.210573405340968,0.315860108011452,0.421146810681936,
0.522142632548711,0.623138454415486,0.72413427628226,0.825130098149035,
0.930416800819519,1.03570350349,1.16736750597208),.UNSPECIFIED.);
#178=B_SPLINE_CURVE_WITH_KNOTS('',3,(#9441,#9442,#9443,#9444,#9445,#9446,
#9447,#9448,#9449,#9450,#9451,#9452,#9453,#9454,#9455,#9456,#9457,#9458,
#9459,#9460,#9461,#9462),.UNSPECIFIED.,.F.,.F.,(4,2,2,2,2,2,2,2,2,2,4),
(0.0789094028588957,0.210573405340968,0.315860108011452,0.421146810681936,
0.522142632548711,0.623138454415485,0.72413427628226,0.825130098149035,
0.930416800819519,1.03570350349,1.16736750597207),.UNSPECIFIED.);
#179=B_SPLINE_CURVE_WITH_KNOTS('',3,(#9470,#9471,#9472,#9473,#9474,#9475,
#9476,#9477,#9478,#9479,#9480,#9481,#9482,#9483,#9484,#9485,#9486,#9487,
#9488,#9489,#9490,#9491),.UNSPECIFIED.,.F.,.F.,(4,2,2,2,2,2,2,2,2,2,4),
(0.0789094028588958,0.210573405340968,0.315860108011452,0.421146810681936,
0.522142632548711,0.623138454415486,0.72413427628226,0.825130098149035,
0.930416800819519,1.03570350349,1.16736750597208),.UNSPECIFIED.);
#180=B_SPLINE_CURVE_WITH_KNOTS('',3,(#9500,#9501,#9502,#9503,#9504,#9505,
#9506,#9507,#9508,#9509,#9510,#9511,#9512,#9513,#9514,#9515,#9516,#9517,
#9518,#9519,#9520,#9521),.UNSPECIFIED.,.F.,.F.,(4,2,2,2,2,2,2,2,2,2,4),
(0.0789094028588958,0.210573405340968,0.315860108011452,0.421146810681936,
0.522142632548711,0.623138454415485,0.72413427628226,0.825130098149035,
0.930416800819519,1.03570350349,1.16736750597208),.UNSPECIFIED.);
#181=B_SPLINE_CURVE_WITH_KNOTS('',3,(#9804,#9805,#9806,#9807,#9808,#9809,
#9810,#9811,#9812,#9813,#9814,#9815,#9816,#9817),.UNSPECIFIED.,.F.,.F.,
(4,2,2,2,2,2,4),(0.756005737987012,0.793568827564648,0.872922520054202,
0.952276212543757,1.03162990503331,1.11098359752287,1.1485466871005),
 .UNSPECIFIED.);
#182=B_SPLINE_CURVE_WITH_KNOTS('',3,(#9823,#9824,#9825,#9826,#9827,#9828,
#9829,#9830,#9831,#9832,#9833,#9834,#9835,#9836,#9837,#9838,#9839,#9840),
 .UNSPECIFIED.,.F.,.F.,(4,2,2,2,2,2,2,2,4),(0.,0.0792165807733632,0.158433161546726,
0.237648697074571,0.316864232602415,0.396079768130259,0.475295303658103,
0.554511884431466,0.63372846520483),.UNSPECIFIED.);
#183=B_SPLINE_CURVE_WITH_KNOTS('',3,(#9841,#9842,#9843,#9844,#9845,#9846,
#9847,#9848,#9849,#9850,#9851,#9852,#9853,#9854,#9855,#9856,#9857,#9858),
 .UNSPECIFIED.,.F.,.F.,(4,2,2,2,2,2,2,2,4),(0.63372846520483,0.712945045978192,
0.792161626751555,0.8713771622794,0.950592697807244,1.02980823333509,1.10902376886293,
1.1882403496363,1.26745693040966),.UNSPECIFIED.);
#184=B_SPLINE_CURVE_WITH_KNOTS('',3,(#9861,#9862,#9863,#9864,#9865,#9866,
#9867,#9868,#9869,#9870,#9871,#9872,#9873,#9874),.UNSPECIFIED.,.F.,.F.,
(4,2,2,2,2,2,4),(0.121154929624506,0.158718019202143,0.238071711691698,
0.317425404181252,0.396779096670807,0.476132789160362,0.513695878738),
 .UNSPECIFIED.);
#185=B_SPLINE_CURVE_WITH_KNOTS('',3,(#9899,#9900,#9901,#9902,#9903,#9904,
#9905,#9906,#9907,#9908),.UNSPECIFIED.,.F.,.F.,(4,2,2,2,4),(0.818088904349169,
0.878131747417166,0.957937926194037,1.03774410497091,1.0977869480389),
 .UNSPECIFIED.);
#186=B_SPLINE_CURVE_WITH_KNOTS('',3,(#9914,#9915,#9916,#9917,#9918,#9919,
#9920,#9921,#9922,#9923,#9924,#9925,#9926,#9927,#9928,#9929,#9930,#9931),
 .UNSPECIFIED.,.F.,.F.,(4,2,2,2,2,2,2,2,4),(0.,0.0792812130427884,0.158562426085577,
0.237841058284634,0.317119690483692,0.396398322682749,0.475676954881807,
0.554958167924595,0.634239380967384),.UNSPECIFIED.);
#187=B_SPLINE_CURVE_WITH_KNOTS('',3,(#9932,#9933,#9934,#9935,#9936,#9937,
#9938,#9939,#9940,#9941,#9942,#9943,#9944,#9945,#9946,#9947,#9948,#9949),
 .UNSPECIFIED.,.F.,.F.,(4,2,2,2,2,2,2,2,4),(0.634239380967384,0.713520594010172,
0.792801807052961,0.872080439252018,0.951359071451076,1.03063770365013,
1.10991633584919,1.18919754889198,1.26847876193477),.UNSPECIFIED.);
#188=B_SPLINE_CURVE_WITH_KNOTS('',3,(#9952,#9953,#9954,#9955,#9956,#9957,
#9958,#9959,#9960,#9961),.UNSPECIFIED.,.F.,.F.,(4,2,2,2,4),(0.17946362021981,
0.239506463287808,0.319312642064679,0.39911882084155,0.459161663909547),
 .UNSPECIFIED.);
#189=B_SPLINE_CURVE_WITH_KNOTS('',3,(#10010,#10011,#10012,#10013,#10014,
#10015,#10016,#10017,#10018,#10019,#10020,#10021,#10022,#10023,#10024,#10025,
#10026,#10027),.UNSPECIFIED.,.F.,.F.,(4,2,2,2,2,2,2,2,4),(0.,0.0472365751919841,
0.0944731503839683,0.14170659898184,0.188940047579712,0.236173496177583,
0.283406944775455,0.330643519967439,0.377880095159423),.UNSPECIFIED.);
#190=B_SPLINE_CURVE_WITH_KNOTS('',3,(#10028,#10029,#10030,#10031,#10032,
#10033,#10034,#10035,#10036,#10037,#10038,#10039,#10040,#10041,#10042,#10043,
#10044,#10045),.UNSPECIFIED.,.F.,.F.,(4,2,2,2,2,2,2,2,4),(0.377880095159423,
0.425116670351408,0.472353245543392,0.519586694141263,0.566820142739135,
0.614053591337007,0.661287039934879,0.708523615126863,0.755760190318847),
 .UNSPECIFIED.);
#191=B_SPLINE_CURVE_WITH_KNOTS('',3,(#10048,#10049,#10050,#10051,#10052,
#10053,#10054,#10055,#10056,#10057,#10058,#10059,#10060,#10061,#10062,#10063,
#10064,#10065),.UNSPECIFIED.,.F.,.F.,(4,2,2,2,2,2,2,2,4),(0.,0.0472365751919841,
0.0944731503839682,0.14170659898184,0.188940047579712,0.236173496177583,
0.283406944775455,0.330643519967439,0.377880095159423),.UNSPECIFIED.);
#192=B_SPLINE_CURVE_WITH_KNOTS('',3,(#10066,#10067,#10068,#10069,#10070,
#10071,#10072,#10073,#10074,#10075,#10076,#10077,#10078,#10079,#10080,#10081,
#10082,#10083),.UNSPECIFIED.,.F.,.F.,(4,2,2,2,2,2,2,2,4),(0.377880095159423,
0.425116670351408,0.472353245543392,0.519586694141263,0.566820142739135,
0.614053591337007,0.661287039934879,0.708523615126863,0.755760190318847),
 .UNSPECIFIED.);
#193=B_SPLINE_CURVE_WITH_KNOTS('',3,(#10086,#10087,#10088,#10089,#10090,
#10091,#10092,#10093,#10094,#10095,#10096,#10097,#10098,#10099,#10100,#10101,
#10102,#10103),.UNSPECIFIED.,.F.,.F.,(4,2,2,2,2,2,2,2,4),(0.,0.0472365751919841,
0.0944731503839683,0.14170659898184,0.188940047579712,0.236173496177583,
0.283406944775455,0.330643519967439,0.377880095159423),.UNSPECIFIED.);
#194=B_SPLINE_CURVE_WITH_KNOTS('',3,(#10104,#10105,#10106,#10107,#10108,
#10109,#10110,#10111,#10112,#10113,#10114,#10115,#10116,#10117,#10118,#10119,
#10120,#10121),.UNSPECIFIED.,.F.,.F.,(4,2,2,2,2,2,2,2,4),(0.377880095159423,
0.425116670351408,0.472353245543392,0.519586694141263,0.566820142739135,
0.614053591337007,0.661287039934879,0.708523615126863,0.755760190318847),
 .UNSPECIFIED.);
#195=B_SPLINE_CURVE_WITH_KNOTS('',3,(#10125,#10126,#10127,#10128,#10129,
#10130,#10131,#10132,#10133,#10134),.UNSPECIFIED.,.F.,.F.,(4,2,2,2,4),(0.565665723963061,
0.61280433739166,0.659942950820258,0.70708195805217,0.754220965284082),
 .UNSPECIFIED.);
#196=B_SPLINE_CURVE_WITH_KNOTS('',3,(#10136,#10137,#10138,#10139,#10140,
#10141,#10142,#10143,#10144,#10145,#10146,#10147,#10148,#10149,#10150,#10151,
#10152,#10153),.UNSPECIFIED.,.F.,.F.,(4,2,2,2,2,2,2,2,4),(0.18855524132102,
0.235693854749619,0.282832468178217,0.329971475410129,0.377110482642041,
0.424249489873953,0.471388497105864,0.518527110534463,0.565665723963061),
 .UNSPECIFIED.);
#197=B_SPLINE_CURVE_WITH_KNOTS('',3,(#10154,#10155,#10156,#10157,#10158,
#10159,#10160,#10161,#10162,#10163),.UNSPECIFIED.,.F.,.F.,(4,2,2,2,4),(0.754220965284082,
0.801359972515993,0.848498979747905,0.895637593176504,0.942776206605102),
 .UNSPECIFIED.);
#198=B_SPLINE_CURVE_WITH_KNOTS('',3,(#10169,#10170,#10171,#10172,#10173,
#10174,#10175,#10176,#10177,#10178),.UNSPECIFIED.,.F.,.F.,(4,2,2,2,4),(0.565665723963061,
0.61280433739166,0.659942950820258,0.70708195805217,0.754220965284082),
 .UNSPECIFIED.);
#199=B_SPLINE_CURVE_WITH_KNOTS('',3,(#10180,#10181,#10182,#10183,#10184,
#10185,#10186,#10187,#10188,#10189,#10190,#10191,#10192,#10193,#10194,#10195,
#10196,#10197),.UNSPECIFIED.,.F.,.F.,(4,2,2,2,2,2,2,2,4),(0.18855524132102,
0.235693854749619,0.282832468178217,0.329971475410129,0.377110482642041,
0.424249489873953,0.471388497105864,0.518527110534463,0.565665723963061),
 .UNSPECIFIED.);
#200=B_SPLINE_CURVE_WITH_KNOTS('',3,(#10198,#10199,#10200,#10201,#10202,
#10203,#10204,#10205,#10206,#10207),.UNSPECIFIED.,.F.,.F.,(4,2,2,2,4),(0.754220965284082,
0.801359972515993,0.848498979747905,0.895637593176504,0.942776206605102),
 .UNSPECIFIED.);
#201=B_SPLINE_CURVE_WITH_KNOTS('',3,(#10217,#10218,#10219,#10220,#10221,
#10222,#10223,#10224,#10225,#10226,#10227,#10228,#10229,#10230,#10231,#10232,
#10233,#10234),.UNSPECIFIED.,.F.,.F.,(4,2,2,2,2,2,2,2,4),(0.18855524132102,
0.235693854749619,0.282832468178217,0.329971475410129,0.377110482642041,
0.424249489873953,0.471388497105864,0.518527110534463,0.565665723963061),
 .UNSPECIFIED.);
#202=B_SPLINE_CURVE_WITH_KNOTS('',3,(#10236,#10237,#10238,#10239,#10240,
#10241,#10242,#10243,#10244,#10245),.UNSPECIFIED.,.F.,.F.,(4,2,2,2,4),(0.565665723963061,
0.61280433739166,0.659942950820258,0.70708195805217,0.754220965284082),
 .UNSPECIFIED.);
#203=B_SPLINE_CURVE_WITH_KNOTS('',3,(#10246,#10247,#10248,#10249,#10250,
#10251,#10252,#10253,#10254,#10255),.UNSPECIFIED.,.F.,.F.,(4,2,2,2,4),(0.754220965284082,
0.801359972515993,0.848498979747905,0.895637593176504,0.942776206605102),
 .UNSPECIFIED.);
#204=B_SPLINE_CURVE_WITH_KNOTS('',3,(#10258,#10259,#10260,#10261,#10262,
#10263,#10264,#10265,#10266,#10267,#10268,#10269,#10270,#10271,#10272,#10273,
#10274,#10275),.UNSPECIFIED.,.F.,.F.,(4,2,2,2,2,2,2,2,4),(0.18855524132102,
0.235693854749619,0.282832468178217,0.329971475410129,0.377110482642041,
0.424249489873953,0.471388497105864,0.518527110534463,0.565665723963061),
 .UNSPECIFIED.);
#205=B_SPLINE_CURVE_WITH_KNOTS('',3,(#10277,#10278,#10279,#10280,#10281,
#10282,#10283,#10284,#10285,#10286),.UNSPECIFIED.,.F.,.F.,(4,2,2,2,4),(0.565665723963061,
0.61280433739166,0.659942950820258,0.70708195805217,0.754220965284082),
 .UNSPECIFIED.);
#206=B_SPLINE_CURVE_WITH_KNOTS('',3,(#10287,#10288,#10289,#10290,#10291,
#10292,#10293,#10294,#10295,#10296),.UNSPECIFIED.,.F.,.F.,(4,2,2,2,4),(0.754220965284082,
0.801359972515993,0.848498979747905,0.895637593176504,0.942776206605102),
 .UNSPECIFIED.);
#207=SPHERICAL_SURFACE('',#6153,0.3969);
#208=SPHERICAL_SURFACE('',#6155,0.3969);
#209=SPHERICAL_SURFACE('',#6157,0.3969);
#210=SPHERICAL_SURFACE('',#6159,0.3969);
#211=SPHERICAL_SURFACE('',#6161,0.3969);
#212=SPHERICAL_SURFACE('',#6163,0.3969);
#213=SPHERICAL_SURFACE('',#6165,0.3969);
#214=SPHERICAL_SURFACE('',#6167,0.3969);
#215=SPHERICAL_SURFACE('',#6170,0.412776);
#216=SPHERICAL_SURFACE('',#6186,0.412776);
#217=SPHERICAL_SURFACE('',#6191,0.412776);
#218=SPHERICAL_SURFACE('',#6196,0.412776);
#219=SPHERICAL_SURFACE('',#6201,0.412776);
#220=SPHERICAL_SURFACE('',#6206,0.412776);
#221=SPHERICAL_SURFACE('',#6211,0.412776);
#222=SPHERICAL_SURFACE('',#6219,0.412776);
#223=CONICAL_SURFACE('',#6124,1.05,0.785398163397449);
#224=CONICAL_SURFACE('',#6131,1.05,0.785398163397449);
#225=CONICAL_SURFACE('',#6144,2.3,0.785398163397449);
#226=CONICAL_SURFACE('',#6148,2.3,0.785398163397449);
#227=CONICAL_SURFACE('',#6248,0.475,0.785398163397449);
#228=CONICAL_SURFACE('',#6252,0.485,0.785398163397448);
#229=CONICAL_SURFACE('',#6256,0.31,0.463647609000806);
#230=CONICAL_SURFACE('',#6260,0.27,0.785398163397448);
#231=CONICAL_SURFACE('',#6274,0.325,0.785398163397448);
#232=CONICAL_SURFACE('',#6278,0.335,0.785398163397448);
#233=CONICAL_SURFACE('',#6282,0.21,0.463647609000806);
#234=CONICAL_SURFACE('',#6286,0.18,0.785398163397448);
#235=CONICAL_SURFACE('',#6671,0.235,0.785398163397448);
#236=CONICAL_SURFACE('',#6675,0.2125,0.785398163397448);
#237=TOROIDAL_SURFACE('',#6113,1.675,0.412776);
#238=TOROIDAL_SURFACE('',#6133,1.675,0.412776);
#239=SHAPE_REPRESENTATION_RELATIONSHIP('SRR','None',#11059,#261);
#240=SHAPE_REPRESENTATION_RELATIONSHIP('SRR','None',#11060,#262);
#241=SHAPE_REPRESENTATION_RELATIONSHIP('SRR','None',#11061,#263);
#242=SHAPE_REPRESENTATION_RELATIONSHIP('SRR','None',#11062,#264);
#243=SHAPE_REPRESENTATION_RELATIONSHIP('SRR','None',#11063,#265);
#244=SHAPE_REPRESENTATION_RELATIONSHIP('SRR','None',#11064,#266);
#245=SHAPE_REPRESENTATION_RELATIONSHIP('SRR','None',#11065,#267);
#246=SHAPE_REPRESENTATION_RELATIONSHIP('SRR','None',#11066,#268);
#247=SHAPE_REPRESENTATION_RELATIONSHIP('SRR','None',#11068,#269);
#248=SHAPE_REPRESENTATION_RELATIONSHIP('SRR','None',#11069,#270);
#249=SHAPE_REPRESENTATION_RELATIONSHIP('SRR','None',#11070,#271);
#250=SHAPE_REPRESENTATION_RELATIONSHIP('SRR','None',#11071,#272);
#251=SHAPE_REPRESENTATION_RELATIONSHIP('SRR','None',#11072,#273);
#252=SHAPE_REPRESENTATION_RELATIONSHIP('SRR','None',#11073,#274);
#253=SHAPE_REPRESENTATION_RELATIONSHIP('SRR','None',#11074,#275);
#254=SHAPE_REPRESENTATION_RELATIONSHIP('SRR','None',#11076,#276);
#255=SHAPE_REPRESENTATION_RELATIONSHIP('SRR','None',#11077,#277);
#256=SHAPE_REPRESENTATION_RELATIONSHIP('SRR','None',#11078,#278);
#257=SHAPE_REPRESENTATION_RELATIONSHIP('SRR','None',#11079,#279);
#258=SHAPE_REPRESENTATION_RELATIONSHIP('SRR','None',#11080,#280);
#259=SHAPE_REPRESENTATION_RELATIONSHIP('SRR','None',#11081,#281);
#260=SHAPE_REPRESENTATION_RELATIONSHIP('SRR','None',#11082,#282);
#261=ADVANCED_BREP_SHAPE_REPRESENTATION('',(#313),#10939);
#262=ADVANCED_BREP_SHAPE_REPRESENTATION('',(#314),#10940);
#263=ADVANCED_BREP_SHAPE_REPRESENTATION('',(#315),#10941);
#264=ADVANCED_BREP_SHAPE_REPRESENTATION('',(#316),#10942);
#265=ADVANCED_BREP_SHAPE_REPRESENTATION('',(#317),#10943);
#266=ADVANCED_BREP_SHAPE_REPRESENTATION('',(#318),#10944);
#267=ADVANCED_BREP_SHAPE_REPRESENTATION('',(#319),#10945);
#268=ADVANCED_BREP_SHAPE_REPRESENTATION('',(#320),#10946);
#269=ADVANCED_BREP_SHAPE_REPRESENTATION('',(#321),#10948);
#270=ADVANCED_BREP_SHAPE_REPRESENTATION('',(#322),#10949);
#271=ADVANCED_BREP_SHAPE_REPRESENTATION('',(#323,#324,#325,#326,#327,#328,
#329,#330),#10950);
#272=ADVANCED_BREP_SHAPE_REPRESENTATION('',(#331),#10951);
#273=ADVANCED_BREP_SHAPE_REPRESENTATION('',(#332,#333),#10952);
#274=ADVANCED_BREP_SHAPE_REPRESENTATION('',(#13),#10953);
#275=ADVANCED_BREP_SHAPE_REPRESENTATION('',(#14),#10954);
#276=ADVANCED_BREP_SHAPE_REPRESENTATION('',(#334),#10956);
#277=ADVANCED_BREP_SHAPE_REPRESENTATION('',(#335),#10957);
#278=ADVANCED_BREP_SHAPE_REPRESENTATION('',(#336),#10958);
#279=ADVANCED_BREP_SHAPE_REPRESENTATION('',(#337),#10959);
#280=ADVANCED_BREP_SHAPE_REPRESENTATION('',(#338),#10960);
#281=ADVANCED_BREP_SHAPE_REPRESENTATION('',(#339),#10961);
#282=ADVANCED_BREP_SHAPE_REPRESENTATION('',(#340),#10962);
#283=STYLED_ITEM('',(#11232),#313);
#284=STYLED_ITEM('',(#11232),#314);
#285=STYLED_ITEM('',(#11253),#315);
#286=STYLED_ITEM('',(#11260),#316);
#287=STYLED_ITEM('',(#11260),#317);
#288=STYLED_ITEM('',(#11246),#318);
#289=STYLED_ITEM('',(#11232),#319);
#290=STYLED_ITEM('',(#11232),#320);
#291=STYLED_ITEM('',(#11253),#321);
#292=STYLED_ITEM('',(#11253),#322);
#293=STYLED_ITEM('',(#11253),#323);
#294=STYLED_ITEM('',(#11253),#324);
#295=STYLED_ITEM('',(#11253),#325);
#296=STYLED_ITEM('',(#11253),#326);
#297=STYLED_ITEM('',(#11253),#327);
#298=STYLED_ITEM('',(#11253),#328);
#299=STYLED_ITEM('',(#11253),#329);
#300=STYLED_ITEM('',(#11253),#330);
#301=STYLED_ITEM('',(#11253),#331);
#302=STYLED_ITEM('',(#11253),#332);
#303=STYLED_ITEM('',(#11253),#333);
#304=STYLED_ITEM('',(#11260),#13);
#305=STYLED_ITEM('',(#11260),#14);
#306=STYLED_ITEM('',(#11253),#334);
#307=STYLED_ITEM('',(#11253),#335);
#308=STYLED_ITEM('',(#11253),#336);
#309=STYLED_ITEM('',(#11267),#337);
#310=STYLED_ITEM('',(#11246),#338);
#311=STYLED_ITEM('',(#11253),#339);
#312=STYLED_ITEM('',(#11260),#340);
#313=MANIFOLD_SOLID_BREP('Body1',#5650);
#314=MANIFOLD_SOLID_BREP('Body1',#5651);
#315=MANIFOLD_SOLID_BREP('Body1',#5652);
#316=MANIFOLD_SOLID_BREP('Body1',#5653);
#317=MANIFOLD_SOLID_BREP('Body1',#5654);
#318=MANIFOLD_SOLID_BREP('Body1',#5655);
#319=MANIFOLD_SOLID_BREP('Body1',#5656);
#320=MANIFOLD_SOLID_BREP('Body1',#5657);
#321=MANIFOLD_SOLID_BREP('Body1',#5658);
#322=MANIFOLD_SOLID_BREP('Body1',#5659);
#323=MANIFOLD_SOLID_BREP('Body1',#5660);
#324=MANIFOLD_SOLID_BREP('Body2',#5661);
#325=MANIFOLD_SOLID_BREP('Body3',#5662);
#326=MANIFOLD_SOLID_BREP('Body4',#5663);
#327=MANIFOLD_SOLID_BREP('Body5',#5664);
#328=MANIFOLD_SOLID_BREP('Body6',#5665);
#329=MANIFOLD_SOLID_BREP('Body7',#5666);
#330=MANIFOLD_SOLID_BREP('Body8',#5667);
#331=MANIFOLD_SOLID_BREP('Continuous crown cage',#5668);
#332=MANIFOLD_SOLID_BREP('Body1',#5669);
#333=MANIFOLD_SOLID_BREP('Body2',#5670);
#334=MANIFOLD_SOLID_BREP('Body1',#5675);
#335=MANIFOLD_SOLID_BREP('Body1',#5676);
#336=MANIFOLD_SOLID_BREP('Body1',#5677);
#337=MANIFOLD_SOLID_BREP('Body1',#5678);
#338=MANIFOLD_SOLID_BREP('Body1',#5679);
#339=MANIFOLD_SOLID_BREP('Body1',#5680);
#340=MANIFOLD_SOLID_BREP('Body1',#5681);
#341=FACE_BOUND('',#915,.T.);
#342=FACE_BOUND('',#916,.T.);
#343=FACE_BOUND('',#917,.T.);
#344=FACE_BOUND('',#918,.T.);
#345=FACE_BOUND('',#920,.T.);
#346=FACE_BOUND('',#921,.T.);
#347=FACE_BOUND('',#922,.T.);
#348=FACE_BOUND('',#923,.T.);
#349=FACE_BOUND('',#949,.T.);
#350=FACE_BOUND('',#951,.T.);
#351=FACE_BOUND('',#954,.T.);
#352=FACE_BOUND('',#955,.T.);
#353=FACE_BOUND('',#962,.T.);
#354=FACE_BOUND('',#964,.T.);
#355=FACE_BOUND('',#967,.T.);
#356=FACE_BOUND('',#968,.T.);
#357=FACE_BOUND('',#972,.T.);
#358=FACE_BOUND('',#973,.T.);
#359=FACE_BOUND('',#975,.T.);
#360=FACE_BOUND('',#976,.T.);
#361=FACE_BOUND('',#977,.T.);
#362=FACE_BOUND('',#978,.T.);
#363=FACE_BOUND('',#979,.T.);
#364=FACE_BOUND('',#981,.T.);
#365=FACE_BOUND('',#982,.T.);
#366=FACE_BOUND('',#983,.T.);
#367=FACE_BOUND('',#984,.T.);
#368=FACE_BOUND('',#985,.T.);
#369=FACE_BOUND('',#989,.T.);
#370=FACE_BOUND('',#991,.T.);
#371=FACE_BOUND('',#998,.T.);
#372=FACE_BOUND('',#1001,.T.);
#373=FACE_BOUND('',#1005,.T.);
#374=FACE_BOUND('',#1006,.T.);
#375=FACE_BOUND('',#1007,.T.);
#376=FACE_BOUND('',#1008,.T.);
#377=FACE_BOUND('',#1009,.T.);
#378=FACE_BOUND('',#1011,.T.);
#379=FACE_BOUND('',#1012,.T.);
#380=FACE_BOUND('',#1013,.T.);
#381=FACE_BOUND('',#1014,.T.);
#382=FACE_BOUND('',#1015,.T.);
#383=FACE_BOUND('',#1019,.T.);
#384=FACE_BOUND('',#1021,.T.);
#385=FACE_BOUND('',#1028,.T.);
#386=FACE_BOUND('',#1032,.T.);
#387=FACE_BOUND('',#1033,.T.);
#388=FACE_BOUND('',#1034,.T.);
#389=FACE_BOUND('',#1035,.T.);
#390=FACE_BOUND('',#1036,.T.);
#391=FACE_BOUND('',#1038,.T.);
#392=FACE_BOUND('',#1039,.T.);
#393=FACE_BOUND('',#1040,.T.);
#394=FACE_BOUND('',#1041,.T.);
#395=FACE_BOUND('',#1042,.T.);
#396=FACE_BOUND('',#1060,.T.);
#397=FACE_BOUND('',#1063,.T.);
#398=FACE_BOUND('',#1068,.T.);
#399=FACE_BOUND('',#1073,.T.);
#400=FACE_BOUND('',#1101,.T.);
#401=FACE_BOUND('',#1104,.T.);
#402=FACE_BOUND('',#1107,.T.);
#403=FACE_BOUND('',#1110,.T.);
#404=FACE_BOUND('',#1113,.T.);
#405=FACE_BOUND('',#1120,.T.);
#406=FACE_BOUND('',#1138,.T.);
#407=FACE_BOUND('',#1157,.T.);
#408=FACE_BOUND('',#1160,.T.);
#409=FACE_BOUND('',#1162,.T.);
#410=FACE_BOUND('',#1167,.T.);
#411=FACE_BOUND('',#1172,.T.);
#412=FACE_BOUND('',#1174,.T.);
#413=FACE_BOUND('',#1179,.T.);
#414=FACE_BOUND('',#1181,.T.);
#415=FACE_BOUND('',#1183,.T.);
#416=FACE_BOUND('',#1185,.T.);
#417=FACE_BOUND('',#1190,.T.);
#418=FACE_BOUND('',#1192,.T.);
#419=FACE_BOUND('',#1194,.T.);
#420=FACE_BOUND('',#1196,.T.);
#421=FACE_BOUND('',#1199,.T.);
#422=FACE_BOUND('',#1202,.T.);
#423=FACE_BOUND('',#1204,.T.);
#424=FACE_BOUND('',#1205,.T.);
#425=FACE_BOUND('',#1206,.T.);
#426=FACE_BOUND('',#1210,.T.);
#427=FACE_BOUND('',#1211,.T.);
#428=FACE_BOUND('',#1212,.T.);
#429=FACE_BOUND('',#1216,.T.);
#430=FACE_BOUND('',#1218,.T.);
#431=FACE_BOUND('',#1221,.T.);
#432=FACE_BOUND('',#1223,.T.);
#433=FACE_BOUND('',#1323,.T.);
#434=PLANE('',#5940);
#435=PLANE('',#5941);
#436=PLANE('',#5942);
#437=PLANE('',#5943);
#438=PLANE('',#5944);
#439=PLANE('',#5945);
#440=PLANE('',#5950);
#441=PLANE('',#5954);
#442=PLANE('',#5958);
#443=PLANE('',#5962);
#444=PLANE('',#5966);
#445=PLANE('',#5970);
#446=PLANE('',#5974);
#447=PLANE('',#5978);
#448=PLANE('',#5991);
#449=PLANE('',#5993);
#450=PLANE('',#5995);
#451=PLANE('',#5997);
#452=PLANE('',#5999);
#453=PLANE('',#6000);
#454=PLANE('',#6001);
#455=PLANE('',#6002);
#456=PLANE('',#6003);
#457=PLANE('',#6004);
#458=PLANE('',#6006);
#459=PLANE('',#6008);
#460=PLANE('',#6010);
#461=PLANE('',#6012);
#462=PLANE('',#6013);
#463=PLANE('',#6014);
#464=PLANE('',#6015);
#465=PLANE('',#6016);
#466=PLANE('',#6023);
#467=PLANE('',#6024);
#468=PLANE('',#6032);
#469=PLANE('',#6033);
#470=PLANE('',#6050);
#471=PLANE('',#6055);
#472=PLANE('',#6061);
#473=PLANE('',#6062);
#474=PLANE('',#6070);
#475=PLANE('',#6071);
#476=PLANE('',#6088);
#477=PLANE('',#6095);
#478=PLANE('',#6096);
#479=PLANE('',#6098);
#480=PLANE('',#6099);
#481=PLANE('',#6100);
#482=PLANE('',#6101);
#483=PLANE('',#6102);
#484=PLANE('',#6103);
#485=PLANE('',#6105);
#486=PLANE('',#6106);
#487=PLANE('',#6107);
#488=PLANE('',#6108);
#489=PLANE('',#6109);
#490=PLANE('',#6110);
#491=PLANE('',#6126);
#492=PLANE('',#6129);
#493=PLANE('',#6141);
#494=PLANE('',#6150);
#495=PLANE('',#6183);
#496=PLANE('',#6188);
#497=PLANE('',#6193);
#498=PLANE('',#6198);
#499=PLANE('',#6203);
#500=PLANE('',#6208);
#501=PLANE('',#6217);
#502=PLANE('',#6221);
#503=PLANE('',#6222);
#504=PLANE('',#6224);
#505=PLANE('',#6229);
#506=PLANE('',#6232);
#507=PLANE('',#6237);
#508=PLANE('',#6246);
#509=PLANE('',#6254);
#510=PLANE('',#6262);
#511=PLANE('',#6263);
#512=PLANE('',#6264);
#513=PLANE('',#6265);
#514=PLANE('',#6266);
#515=PLANE('',#6267);
#516=PLANE('',#6268);
#517=PLANE('',#6269);
#518=PLANE('',#6270);
#519=PLANE('',#6272);
#520=PLANE('',#6280);
#521=PLANE('',#6288);
#522=PLANE('',#6289);
#523=PLANE('',#6290);
#524=PLANE('',#6291);
#525=PLANE('',#6292);
#526=PLANE('',#6293);
#527=PLANE('',#6294);
#528=PLANE('',#6295);
#529=PLANE('',#6296);
#530=PLANE('',#6321);
#531=PLANE('',#6322);
#532=PLANE('',#6324);
#533=PLANE('',#6325);
#534=PLANE('',#6326);
#535=PLANE('',#6331);
#536=PLANE('',#6332);
#537=PLANE('',#6335);
#538=PLANE('',#6343);
#539=PLANE('',#6344);
#540=PLANE('',#6352);
#541=PLANE('',#6353);
#542=PLANE('',#6355);
#543=PLANE('',#6360);
#544=PLANE('',#6367);
#545=PLANE('',#6368);
#546=PLANE('',#6370);
#547=PLANE('',#6375);
#548=PLANE('',#6382);
#549=PLANE('',#6383);
#550=PLANE('',#6385);
#551=PLANE('',#6386);
#552=PLANE('',#6388);
#553=PLANE('',#6389);
#554=PLANE('',#6401);
#555=PLANE('',#6402);
#556=PLANE('',#6486);
#557=PLANE('',#6487);
#558=PLANE('',#6651);
#559=PLANE('',#6652);
#560=PLANE('',#6653);
#561=PLANE('',#6654);
#562=PLANE('',#6655);
#563=PLANE('',#6656);
#564=PLANE('',#6657);
#565=PLANE('',#6658);
#566=PLANE('',#6659);
#567=PLANE('',#6660);
#568=PLANE('',#6662);
#569=PLANE('',#6663);
#570=PLANE('',#6664);
#571=PLANE('',#6665);
#572=PLANE('',#6666);
#573=PLANE('',#6667);
#574=PLANE('',#6668);
#575=PLANE('',#6669);
#576=PLANE('',#6677);
#577=FACE_OUTER_BOUND('',#906,.T.);
#578=FACE_OUTER_BOUND('',#907,.T.);
#579=FACE_OUTER_BOUND('',#908,.T.);
#580=FACE_OUTER_BOUND('',#909,.T.);
#581=FACE_OUTER_BOUND('',#910,.T.);
#582=FACE_OUTER_BOUND('',#911,.T.);
#583=FACE_OUTER_BOUND('',#912,.T.);
#584=FACE_OUTER_BOUND('',#913,.T.);
#585=FACE_OUTER_BOUND('',#914,.T.);
#586=FACE_OUTER_BOUND('',#919,.T.);
#587=FACE_OUTER_BOUND('',#924,.T.);
#588=FACE_OUTER_BOUND('',#925,.T.);
#589=FACE_OUTER_BOUND('',#926,.T.);
#590=FACE_OUTER_BOUND('',#927,.T.);
#591=FACE_OUTER_BOUND('',#928,.T.);
#592=FACE_OUTER_BOUND('',#929,.T.);
#593=FACE_OUTER_BOUND('',#930,.T.);
#594=FACE_OUTER_BOUND('',#931,.T.);
#595=FACE_OUTER_BOUND('',#932,.T.);
#596=FACE_OUTER_BOUND('',#933,.T.);
#597=FACE_OUTER_BOUND('',#934,.T.);
#598=FACE_OUTER_BOUND('',#935,.T.);
#599=FACE_OUTER_BOUND('',#936,.T.);
#600=FACE_OUTER_BOUND('',#937,.T.);
#601=FACE_OUTER_BOUND('',#938,.T.);
#602=FACE_OUTER_BOUND('',#939,.T.);
#603=FACE_OUTER_BOUND('',#940,.T.);
#604=FACE_OUTER_BOUND('',#941,.T.);
#605=FACE_OUTER_BOUND('',#942,.T.);
#606=FACE_OUTER_BOUND('',#943,.T.);
#607=FACE_OUTER_BOUND('',#944,.T.);
#608=FACE_OUTER_BOUND('',#945,.T.);
#609=FACE_OUTER_BOUND('',#946,.T.);
#610=FACE_OUTER_BOUND('',#947,.T.);
#611=FACE_OUTER_BOUND('',#948,.T.);
#612=FACE_OUTER_BOUND('',#950,.T.);
#613=FACE_OUTER_BOUND('',#952,.T.);
#614=FACE_OUTER_BOUND('',#953,.T.);
#615=FACE_OUTER_BOUND('',#956,.T.);
#616=FACE_OUTER_BOUND('',#957,.T.);
#617=FACE_OUTER_BOUND('',#958,.T.);
#618=FACE_OUTER_BOUND('',#959,.T.);
#619=FACE_OUTER_BOUND('',#960,.T.);
#620=FACE_OUTER_BOUND('',#961,.T.);
#621=FACE_OUTER_BOUND('',#963,.T.);
#622=FACE_OUTER_BOUND('',#965,.T.);
#623=FACE_OUTER_BOUND('',#966,.T.);
#624=FACE_OUTER_BOUND('',#969,.T.);
#625=FACE_OUTER_BOUND('',#970,.T.);
#626=FACE_OUTER_BOUND('',#971,.T.);
#627=FACE_OUTER_BOUND('',#974,.T.);
#628=FACE_OUTER_BOUND('',#980,.T.);
#629=FACE_OUTER_BOUND('',#986,.T.);
#630=FACE_OUTER_BOUND('',#987,.T.);
#631=FACE_OUTER_BOUND('',#988,.T.);
#632=FACE_OUTER_BOUND('',#990,.T.);
#633=FACE_OUTER_BOUND('',#992,.T.);
#634=FACE_OUTER_BOUND('',#993,.T.);
#635=FACE_OUTER_BOUND('',#994,.T.);
#636=FACE_OUTER_BOUND('',#995,.T.);
#637=FACE_OUTER_BOUND('',#996,.T.);
#638=FACE_OUTER_BOUND('',#997,.T.);
#639=FACE_OUTER_BOUND('',#999,.T.);
#640=FACE_OUTER_BOUND('',#1000,.T.);
#641=FACE_OUTER_BOUND('',#1002,.T.);
#642=FACE_OUTER_BOUND('',#1003,.T.);
#643=FACE_OUTER_BOUND('',#1004,.T.);
#644=FACE_OUTER_BOUND('',#1010,.T.);
#645=FACE_OUTER_BOUND('',#1016,.T.);
#646=FACE_OUTER_BOUND('',#1017,.T.);
#647=FACE_OUTER_BOUND('',#1018,.T.);
#648=FACE_OUTER_BOUND('',#1020,.T.);
#649=FACE_OUTER_BOUND('',#1022,.T.);
#650=FACE_OUTER_BOUND('',#1023,.T.);
#651=FACE_OUTER_BOUND('',#1024,.T.);
#652=FACE_OUTER_BOUND('',#1025,.T.);
#653=FACE_OUTER_BOUND('',#1026,.T.);
#654=FACE_OUTER_BOUND('',#1027,.T.);
#655=FACE_OUTER_BOUND('',#1029,.T.);
#656=FACE_OUTER_BOUND('',#1030,.T.);
#657=FACE_OUTER_BOUND('',#1031,.T.);
#658=FACE_OUTER_BOUND('',#1037,.T.);
#659=FACE_OUTER_BOUND('',#1043,.T.);
#660=FACE_OUTER_BOUND('',#1044,.T.);
#661=FACE_OUTER_BOUND('',#1045,.T.);
#662=FACE_OUTER_BOUND('',#1046,.T.);
#663=FACE_OUTER_BOUND('',#1047,.T.);
#664=FACE_OUTER_BOUND('',#1048,.T.);
#665=FACE_OUTER_BOUND('',#1049,.T.);
#666=FACE_OUTER_BOUND('',#1050,.T.);
#667=FACE_OUTER_BOUND('',#1051,.T.);
#668=FACE_OUTER_BOUND('',#1052,.T.);
#669=FACE_OUTER_BOUND('',#1053,.T.);
#670=FACE_OUTER_BOUND('',#1054,.T.);
#671=FACE_OUTER_BOUND('',#1055,.T.);
#672=FACE_OUTER_BOUND('',#1056,.T.);
#673=FACE_OUTER_BOUND('',#1057,.T.);
#674=FACE_OUTER_BOUND('',#1058,.T.);
#675=FACE_OUTER_BOUND('',#1059,.T.);
#676=FACE_OUTER_BOUND('',#1061,.T.);
#677=FACE_OUTER_BOUND('',#1062,.T.);
#678=FACE_OUTER_BOUND('',#1064,.T.);
#679=FACE_OUTER_BOUND('',#1065,.T.);
#680=FACE_OUTER_BOUND('',#1066,.T.);
#681=FACE_OUTER_BOUND('',#1067,.T.);
#682=FACE_OUTER_BOUND('',#1069,.T.);
#683=FACE_OUTER_BOUND('',#1070,.T.);
#684=FACE_OUTER_BOUND('',#1071,.T.);
#685=FACE_OUTER_BOUND('',#1072,.T.);
#686=FACE_OUTER_BOUND('',#1074,.T.);
#687=FACE_OUTER_BOUND('',#1075,.T.);
#688=FACE_OUTER_BOUND('',#1076,.T.);
#689=FACE_OUTER_BOUND('',#1077,.T.);
#690=FACE_OUTER_BOUND('',#1078,.T.);
#691=FACE_OUTER_BOUND('',#1079,.T.);
#692=FACE_OUTER_BOUND('',#1080,.T.);
#693=FACE_OUTER_BOUND('',#1081,.T.);
#694=FACE_OUTER_BOUND('',#1082,.T.);
#695=FACE_OUTER_BOUND('',#1083,.T.);
#696=FACE_OUTER_BOUND('',#1084,.T.);
#697=FACE_OUTER_BOUND('',#1085,.T.);
#698=FACE_OUTER_BOUND('',#1086,.T.);
#699=FACE_OUTER_BOUND('',#1087,.T.);
#700=FACE_OUTER_BOUND('',#1088,.T.);
#701=FACE_OUTER_BOUND('',#1089,.T.);
#702=FACE_OUTER_BOUND('',#1090,.T.);
#703=FACE_OUTER_BOUND('',#1091,.T.);
#704=FACE_OUTER_BOUND('',#1092,.T.);
#705=FACE_OUTER_BOUND('',#1093,.T.);
#706=FACE_OUTER_BOUND('',#1094,.T.);
#707=FACE_OUTER_BOUND('',#1095,.T.);
#708=FACE_OUTER_BOUND('',#1096,.T.);
#709=FACE_OUTER_BOUND('',#1097,.T.);
#710=FACE_OUTER_BOUND('',#1098,.T.);
#711=FACE_OUTER_BOUND('',#1099,.T.);
#712=FACE_OUTER_BOUND('',#1100,.T.);
#713=FACE_OUTER_BOUND('',#1102,.T.);
#714=FACE_OUTER_BOUND('',#1103,.T.);
#715=FACE_OUTER_BOUND('',#1105,.T.);
#716=FACE_OUTER_BOUND('',#1106,.T.);
#717=FACE_OUTER_BOUND('',#1108,.T.);
#718=FACE_OUTER_BOUND('',#1109,.T.);
#719=FACE_OUTER_BOUND('',#1111,.T.);
#720=FACE_OUTER_BOUND('',#1112,.T.);
#721=FACE_OUTER_BOUND('',#1114,.T.);
#722=FACE_OUTER_BOUND('',#1115,.T.);
#723=FACE_OUTER_BOUND('',#1116,.T.);
#724=FACE_OUTER_BOUND('',#1117,.T.);
#725=FACE_OUTER_BOUND('',#1118,.T.);
#726=FACE_OUTER_BOUND('',#1119,.T.);
#727=FACE_OUTER_BOUND('',#1121,.T.);
#728=FACE_OUTER_BOUND('',#1122,.T.);
#729=FACE_OUTER_BOUND('',#1123,.T.);
#730=FACE_OUTER_BOUND('',#1124,.T.);
#731=FACE_OUTER_BOUND('',#1125,.T.);
#732=FACE_OUTER_BOUND('',#1126,.T.);
#733=FACE_OUTER_BOUND('',#1127,.T.);
#734=FACE_OUTER_BOUND('',#1128,.T.);
#735=FACE_OUTER_BOUND('',#1129,.T.);
#736=FACE_OUTER_BOUND('',#1130,.T.);
#737=FACE_OUTER_BOUND('',#1131,.T.);
#738=FACE_OUTER_BOUND('',#1132,.T.);
#739=FACE_OUTER_BOUND('',#1133,.T.);
#740=FACE_OUTER_BOUND('',#1134,.T.);
#741=FACE_OUTER_BOUND('',#1135,.T.);
#742=FACE_OUTER_BOUND('',#1136,.T.);
#743=FACE_OUTER_BOUND('',#1137,.T.);
#744=FACE_OUTER_BOUND('',#1139,.T.);
#745=FACE_OUTER_BOUND('',#1140,.T.);
#746=FACE_OUTER_BOUND('',#1141,.T.);
#747=FACE_OUTER_BOUND('',#1142,.T.);
#748=FACE_OUTER_BOUND('',#1143,.T.);
#749=FACE_OUTER_BOUND('',#1144,.T.);
#750=FACE_OUTER_BOUND('',#1145,.T.);
#751=FACE_OUTER_BOUND('',#1146,.T.);
#752=FACE_OUTER_BOUND('',#1147,.T.);
#753=FACE_OUTER_BOUND('',#1148,.T.);
#754=FACE_OUTER_BOUND('',#1149,.T.);
#755=FACE_OUTER_BOUND('',#1150,.T.);
#756=FACE_OUTER_BOUND('',#1151,.T.);
#757=FACE_OUTER_BOUND('',#1152,.T.);
#758=FACE_OUTER_BOUND('',#1153,.T.);
#759=FACE_OUTER_BOUND('',#1154,.T.);
#760=FACE_OUTER_BOUND('',#1155,.T.);
#761=FACE_OUTER_BOUND('',#1156,.T.);
#762=FACE_OUTER_BOUND('',#1158,.T.);
#763=FACE_OUTER_BOUND('',#1159,.T.);
#764=FACE_OUTER_BOUND('',#1161,.T.);
#765=FACE_OUTER_BOUND('',#1163,.T.);
#766=FACE_OUTER_BOUND('',#1164,.T.);
#767=FACE_OUTER_BOUND('',#1165,.T.);
#768=FACE_OUTER_BOUND('',#1166,.T.);
#769=FACE_OUTER_BOUND('',#1168,.T.);
#770=FACE_OUTER_BOUND('',#1169,.T.);
#771=FACE_OUTER_BOUND('',#1170,.T.);
#772=FACE_OUTER_BOUND('',#1171,.T.);
#773=FACE_OUTER_BOUND('',#1173,.T.);
#774=FACE_OUTER_BOUND('',#1175,.T.);
#775=FACE_OUTER_BOUND('',#1176,.T.);
#776=FACE_OUTER_BOUND('',#1177,.T.);
#777=FACE_OUTER_BOUND('',#1178,.T.);
#778=FACE_OUTER_BOUND('',#1180,.T.);
#779=FACE_OUTER_BOUND('',#1182,.T.);
#780=FACE_OUTER_BOUND('',#1184,.T.);
#781=FACE_OUTER_BOUND('',#1186,.T.);
#782=FACE_OUTER_BOUND('',#1187,.T.);
#783=FACE_OUTER_BOUND('',#1188,.T.);
#784=FACE_OUTER_BOUND('',#1189,.T.);
#785=FACE_OUTER_BOUND('',#1191,.T.);
#786=FACE_OUTER_BOUND('',#1193,.T.);
#787=FACE_OUTER_BOUND('',#1195,.T.);
#788=FACE_OUTER_BOUND('',#1197,.T.);
#789=FACE_OUTER_BOUND('',#1198,.T.);
#790=FACE_OUTER_BOUND('',#1200,.T.);
#791=FACE_OUTER_BOUND('',#1201,.T.);
#792=FACE_OUTER_BOUND('',#1203,.T.);
#793=FACE_OUTER_BOUND('',#1207,.T.);
#794=FACE_OUTER_BOUND('',#1208,.T.);
#795=FACE_OUTER_BOUND('',#1209,.T.);
#796=FACE_OUTER_BOUND('',#1213,.T.);
#797=FACE_OUTER_BOUND('',#1214,.T.);
#798=FACE_OUTER_BOUND('',#1215,.T.);
#799=FACE_OUTER_BOUND('',#1217,.T.);
#800=FACE_OUTER_BOUND('',#1219,.T.);
#801=FACE_OUTER_BOUND('',#1220,.T.);
#802=FACE_OUTER_BOUND('',#1222,.T.);
#803=FACE_OUTER_BOUND('',#1224,.T.);
#804=FACE_OUTER_BOUND('',#1225,.T.);
#805=FACE_OUTER_BOUND('',#1226,.T.);
#806=FACE_OUTER_BOUND('',#1227,.T.);
#807=FACE_OUTER_BOUND('',#1228,.T.);
#808=FACE_OUTER_BOUND('',#1229,.T.);
#809=FACE_OUTER_BOUND('',#1230,.T.);
#810=FACE_OUTER_BOUND('',#1231,.T.);
#811=FACE_OUTER_BOUND('',#1232,.T.);
#812=FACE_OUTER_BOUND('',#1233,.T.);
#813=FACE_OUTER_BOUND('',#1234,.T.);
#814=FACE_OUTER_BOUND('',#1235,.T.);
#815=FACE_OUTER_BOUND('',#1236,.T.);
#816=FACE_OUTER_BOUND('',#1237,.T.);
#817=FACE_OUTER_BOUND('',#1238,.T.);
#818=FACE_OUTER_BOUND('',#1239,.T.);
#819=FACE_OUTER_BOUND('',#1240,.T.);
#820=FACE_OUTER_BOUND('',#1241,.T.);
#821=FACE_OUTER_BOUND('',#1242,.T.);
#822=FACE_OUTER_BOUND('',#1243,.T.);
#823=FACE_OUTER_BOUND('',#1244,.T.);
#824=FACE_OUTER_BOUND('',#1245,.T.);
#825=FACE_OUTER_BOUND('',#1246,.T.);
#826=FACE_OUTER_BOUND('',#1247,.T.);
#827=FACE_OUTER_BOUND('',#1248,.T.);
#828=FACE_OUTER_BOUND('',#1249,.T.);
#829=FACE_OUTER_BOUND('',#1250,.T.);
#830=FACE_OUTER_BOUND('',#1251,.T.);
#831=FACE_OUTER_BOUND('',#1252,.T.);
#832=FACE_OUTER_BOUND('',#1253,.T.);
#833=FACE_OUTER_BOUND('',#1254,.T.);
#834=FACE_OUTER_BOUND('',#1255,.T.);
#835=FACE_OUTER_BOUND('',#1256,.T.);
#836=FACE_OUTER_BOUND('',#1257,.T.);
#837=FACE_OUTER_BOUND('',#1258,.T.);
#838=FACE_OUTER_BOUND('',#1259,.T.);
#839=FACE_OUTER_BOUND('',#1260,.T.);
#840=FACE_OUTER_BOUND('',#1261,.T.);
#841=FACE_OUTER_BOUND('',#1262,.T.);
#842=FACE_OUTER_BOUND('',#1263,.T.);
#843=FACE_OUTER_BOUND('',#1264,.T.);
#844=FACE_OUTER_BOUND('',#1265,.T.);
#845=FACE_OUTER_BOUND('',#1266,.T.);
#846=FACE_OUTER_BOUND('',#1267,.T.);
#847=FACE_OUTER_BOUND('',#1268,.T.);
#848=FACE_OUTER_BOUND('',#1269,.T.);
#849=FACE_OUTER_BOUND('',#1270,.T.);
#850=FACE_OUTER_BOUND('',#1271,.T.);
#851=FACE_OUTER_BOUND('',#1272,.T.);
#852=FACE_OUTER_BOUND('',#1273,.T.);
#853=FACE_OUTER_BOUND('',#1274,.T.);
#854=FACE_OUTER_BOUND('',#1275,.T.);
#855=FACE_OUTER_BOUND('',#1276,.T.);
#856=FACE_OUTER_BOUND('',#1277,.T.);
#857=FACE_OUTER_BOUND('',#1278,.T.);
#858=FACE_OUTER_BOUND('',#1279,.T.);
#859=FACE_OUTER_BOUND('',#1280,.T.);
#860=FACE_OUTER_BOUND('',#1281,.T.);
#861=FACE_OUTER_BOUND('',#1282,.T.);
#862=FACE_OUTER_BOUND('',#1283,.T.);
#863=FACE_OUTER_BOUND('',#1284,.T.);
#864=FACE_OUTER_BOUND('',#1285,.T.);
#865=FACE_OUTER_BOUND('',#1286,.T.);
#866=FACE_OUTER_BOUND('',#1287,.T.);
#867=FACE_OUTER_BOUND('',#1288,.T.);
#868=FACE_OUTER_BOUND('',#1289,.T.);
#869=FACE_OUTER_BOUND('',#1290,.T.);
#870=FACE_OUTER_BOUND('',#1291,.T.);
#871=FACE_OUTER_BOUND('',#1292,.T.);
#872=FACE_OUTER_BOUND('',#1293,.T.);
#873=FACE_OUTER_BOUND('',#1294,.T.);
#874=FACE_OUTER_BOUND('',#1295,.T.);
#875=FACE_OUTER_BOUND('',#1296,.T.);
#876=FACE_OUTER_BOUND('',#1297,.T.);
#877=FACE_OUTER_BOUND('',#1298,.T.);
#878=FACE_OUTER_BOUND('',#1299,.T.);
#879=FACE_OUTER_BOUND('',#1300,.T.);
#880=FACE_OUTER_BOUND('',#1301,.T.);
#881=FACE_OUTER_BOUND('',#1302,.T.);
#882=FACE_OUTER_BOUND('',#1303,.T.);
#883=FACE_OUTER_BOUND('',#1304,.T.);
#884=FACE_OUTER_BOUND('',#1305,.T.);
#885=FACE_OUTER_BOUND('',#1306,.T.);
#886=FACE_OUTER_BOUND('',#1307,.T.);
#887=FACE_OUTER_BOUND('',#1308,.T.);
#888=FACE_OUTER_BOUND('',#1309,.T.);
#889=FACE_OUTER_BOUND('',#1310,.T.);
#890=FACE_OUTER_BOUND('',#1311,.T.);
#891=FACE_OUTER_BOUND('',#1312,.T.);
#892=FACE_OUTER_BOUND('',#1313,.T.);
#893=FACE_OUTER_BOUND('',#1314,.T.);
#894=FACE_OUTER_BOUND('',#1315,.T.);
#895=FACE_OUTER_BOUND('',#1316,.T.);
#896=FACE_OUTER_BOUND('',#1317,.T.);
#897=FACE_OUTER_BOUND('',#1318,.T.);
#898=FACE_OUTER_BOUND('',#1319,.T.);
#899=FACE_OUTER_BOUND('',#1320,.T.);
#900=FACE_OUTER_BOUND('',#1321,.T.);
#901=FACE_OUTER_BOUND('',#1322,.T.);
#902=FACE_OUTER_BOUND('',#1324,.T.);
#903=FACE_OUTER_BOUND('',#1325,.T.);
#904=FACE_OUTER_BOUND('',#1326,.T.);
#905=FACE_OUTER_BOUND('',#1327,.T.);
#906=EDGE_LOOP('',(#3653,#3654,#3655,#3656));
#907=EDGE_LOOP('',(#3657,#3658,#3659,#3660));
#908=EDGE_LOOP('',(#3661,#3662,#3663,#3664));
#909=EDGE_LOOP('',(#3665,#3666,#3667,#3668));
#910=EDGE_LOOP('',(#3669,#3670,#3671,#3672));
#911=EDGE_LOOP('',(#3673,#3674,#3675,#3676));
#912=EDGE_LOOP('',(#3677,#3678,#3679,#3680));
#913=EDGE_LOOP('',(#3681,#3682,#3683,#3684));
#914=EDGE_LOOP('',(#3685,#3686,#3687,#3688));
#915=EDGE_LOOP('',(#3689));
#916=EDGE_LOOP('',(#3690));
#917=EDGE_LOOP('',(#3691));
#918=EDGE_LOOP('',(#3692));
#919=EDGE_LOOP('',(#3693,#3694,#3695,#3696));
#920=EDGE_LOOP('',(#3697));
#921=EDGE_LOOP('',(#3698));
#922=EDGE_LOOP('',(#3699));
#923=EDGE_LOOP('',(#3700));
#924=EDGE_LOOP('',(#3701,#3702,#3703,#3704));
#925=EDGE_LOOP('',(#3705));
#926=EDGE_LOOP('',(#3706,#3707,#3708,#3709));
#927=EDGE_LOOP('',(#3710));
#928=EDGE_LOOP('',(#3711,#3712,#3713,#3714));
#929=EDGE_LOOP('',(#3715));
#930=EDGE_LOOP('',(#3716,#3717,#3718,#3719));
#931=EDGE_LOOP('',(#3720));
#932=EDGE_LOOP('',(#3721,#3722,#3723,#3724));
#933=EDGE_LOOP('',(#3725));
#934=EDGE_LOOP('',(#3726,#3727,#3728,#3729));
#935=EDGE_LOOP('',(#3730));
#936=EDGE_LOOP('',(#3731,#3732,#3733,#3734));
#937=EDGE_LOOP('',(#3735));
#938=EDGE_LOOP('',(#3736,#3737,#3738,#3739));
#939=EDGE_LOOP('',(#3740));
#940=EDGE_LOOP('',(#3741,#3742,#3743,#3744));
#941=EDGE_LOOP('',(#3745,#3746,#3747,#3748));
#942=EDGE_LOOP('',(#3749,#3750,#3751,#3752));
#943=EDGE_LOOP('',(#3753,#3754,#3755,#3756));
#944=EDGE_LOOP('',(#3757,#3758,#3759,#3760));
#945=EDGE_LOOP('',(#3761,#3762,#3763,#3764));
#946=EDGE_LOOP('',(#3765,#3766,#3767,#3768));
#947=EDGE_LOOP('',(#3769,#3770,#3771,#3772));
#948=EDGE_LOOP('',(#3773,#3774,#3775,#3776));
#949=EDGE_LOOP('',(#3777));
#950=EDGE_LOOP('',(#3778,#3779,#3780,#3781));
#951=EDGE_LOOP('',(#3782));
#952=EDGE_LOOP('',(#3783,#3784,#3785,#3786));
#953=EDGE_LOOP('',(#3787,#3788,#3789,#3790,#3791,#3792));
#954=EDGE_LOOP('',(#3793));
#955=EDGE_LOOP('',(#3794));
#956=EDGE_LOOP('',(#3795,#3796,#3797,#3798));
#957=EDGE_LOOP('',(#3799,#3800,#3801,#3802));
#958=EDGE_LOOP('',(#3803,#3804,#3805,#3806));
#959=EDGE_LOOP('',(#3807,#3808,#3809,#3810));
#960=EDGE_LOOP('',(#3811,#3812,#3813,#3814));
#961=EDGE_LOOP('',(#3815,#3816,#3817,#3818));
#962=EDGE_LOOP('',(#3819));
#963=EDGE_LOOP('',(#3820,#3821,#3822,#3823));
#964=EDGE_LOOP('',(#3824));
#965=EDGE_LOOP('',(#3825,#3826,#3827,#3828));
#966=EDGE_LOOP('',(#3829,#3830,#3831,#3832,#3833,#3834));
#967=EDGE_LOOP('',(#3835));
#968=EDGE_LOOP('',(#3836));
#969=EDGE_LOOP('',(#3837,#3838,#3839,#3840));
#970=EDGE_LOOP('',(#3841,#3842,#3843,#3844));
#971=EDGE_LOOP('',(#3845,#3846,#3847,#3848));
#972=EDGE_LOOP('',(#3849,#3850,#3851,#3852,#3853,#3854));
#973=EDGE_LOOP('',(#3855,#3856,#3857,#3858,#3859,#3860));
#974=EDGE_LOOP('',(#3861));
#975=EDGE_LOOP('',(#3862));
#976=EDGE_LOOP('',(#3863));
#977=EDGE_LOOP('',(#3864));
#978=EDGE_LOOP('',(#3865));
#979=EDGE_LOOP('',(#3866));
#980=EDGE_LOOP('',(#3867));
#981=EDGE_LOOP('',(#3868));
#982=EDGE_LOOP('',(#3869));
#983=EDGE_LOOP('',(#3870));
#984=EDGE_LOOP('',(#3871));
#985=EDGE_LOOP('',(#3872));
#986=EDGE_LOOP('',(#3873,#3874,#3875,#3876));
#987=EDGE_LOOP('',(#3877,#3878,#3879,#3880));
#988=EDGE_LOOP('',(#3881));
#989=EDGE_LOOP('',(#3882));
#990=EDGE_LOOP('',(#3883));
#991=EDGE_LOOP('',(#3884));
#992=EDGE_LOOP('',(#3885,#3886,#3887,#3888));
#993=EDGE_LOOP('',(#3889,#3890,#3891,#3892));
#994=EDGE_LOOP('',(#3893,#3894,#3895,#3896));
#995=EDGE_LOOP('',(#3897,#3898,#3899,#3900));
#996=EDGE_LOOP('',(#3901,#3902,#3903,#3904));
#997=EDGE_LOOP('',(#3905));
#998=EDGE_LOOP('',(#3906));
#999=EDGE_LOOP('',(#3907,#3908,#3909,#3910));
#1000=EDGE_LOOP('',(#3911));
#1001=EDGE_LOOP('',(#3912));
#1002=EDGE_LOOP('',(#3913,#3914,#3915,#3916));
#1003=EDGE_LOOP('',(#3917,#3918,#3919,#3920));
#1004=EDGE_LOOP('',(#3921));
#1005=EDGE_LOOP('',(#3922));
#1006=EDGE_LOOP('',(#3923));
#1007=EDGE_LOOP('',(#3924));
#1008=EDGE_LOOP('',(#3925));
#1009=EDGE_LOOP('',(#3926));
#1010=EDGE_LOOP('',(#3927));
#1011=EDGE_LOOP('',(#3928));
#1012=EDGE_LOOP('',(#3929));
#1013=EDGE_LOOP('',(#3930));
#1014=EDGE_LOOP('',(#3931));
#1015=EDGE_LOOP('',(#3932));
#1016=EDGE_LOOP('',(#3933,#3934,#3935,#3936));
#1017=EDGE_LOOP('',(#3937,#3938,#3939,#3940));
#1018=EDGE_LOOP('',(#3941));
#1019=EDGE_LOOP('',(#3942));
#1020=EDGE_LOOP('',(#3943));
#1021=EDGE_LOOP('',(#3944));
#1022=EDGE_LOOP('',(#3945,#3946,#3947,#3948));
#1023=EDGE_LOOP('',(#3949,#3950,#3951,#3952));
#1024=EDGE_LOOP('',(#3953,#3954,#3955,#3956));
#1025=EDGE_LOOP('',(#3957,#3958,#3959,#3960));
#1026=EDGE_LOOP('',(#3961,#3962,#3963,#3964));
#1027=EDGE_LOOP('',(#3965));
#1028=EDGE_LOOP('',(#3966));
#1029=EDGE_LOOP('',(#3967,#3968,#3969,#3970));
#1030=EDGE_LOOP('',(#3971,#3972,#3973,#3974));
#1031=EDGE_LOOP('',(#3975));
#1032=EDGE_LOOP('',(#3976));
#1033=EDGE_LOOP('',(#3977));
#1034=EDGE_LOOP('',(#3978));
#1035=EDGE_LOOP('',(#3979));
#1036=EDGE_LOOP('',(#3980));
#1037=EDGE_LOOP('',(#3981));
#1038=EDGE_LOOP('',(#3982));
#1039=EDGE_LOOP('',(#3983));
#1040=EDGE_LOOP('',(#3984));
#1041=EDGE_LOOP('',(#3985));
#1042=EDGE_LOOP('',(#3986));
#1043=EDGE_LOOP('',(#3987,#3988,#3989,#3990));
#1044=EDGE_LOOP('',(#3991,#3992,#3993,#3994));
#1045=EDGE_LOOP('',(#3995,#3996,#3997,#3998));
#1046=EDGE_LOOP('',(#3999,#4000,#4001,#4002));
#1047=EDGE_LOOP('',(#4003,#4004,#4005,#4006));
#1048=EDGE_LOOP('',(#4007,#4008,#4009,#4010));
#1049=EDGE_LOOP('',(#4011,#4012,#4013,#4014));
#1050=EDGE_LOOP('',(#4015,#4016,#4017,#4018));
#1051=EDGE_LOOP('',(#4019,#4020,#4021,#4022));
#1052=EDGE_LOOP('',(#4023,#4024,#4025,#4026));
#1053=EDGE_LOOP('',(#4027,#4028,#4029,#4030));
#1054=EDGE_LOOP('',(#4031,#4032,#4033,#4034));
#1055=EDGE_LOOP('',(#4035,#4036,#4037,#4038,#4039,#4040));
#1056=EDGE_LOOP('',(#4041,#4042,#4043,#4044,#4045));
#1057=EDGE_LOOP('',(#4046,#4047,#4048,#4049));
#1058=EDGE_LOOP('',(#4050,#4051,#4052,#4053));
#1059=EDGE_LOOP('',(#4054));
#1060=EDGE_LOOP('',(#4055));
#1061=EDGE_LOOP('',(#4056,#4057,#4058,#4059,#4060));
#1062=EDGE_LOOP('',(#4061));
#1063=EDGE_LOOP('',(#4062));
#1064=EDGE_LOOP('',(#4063,#4064,#4065,#4066));
#1065=EDGE_LOOP('',(#4067,#4068,#4069,#4070,#4071,#4072));
#1066=EDGE_LOOP('',(#4073,#4074,#4075,#4076,#4077));
#1067=EDGE_LOOP('',(#4078));
#1068=EDGE_LOOP('',(#4079));
#1069=EDGE_LOOP('',(#4080,#4081,#4082,#4083));
#1070=EDGE_LOOP('',(#4084,#4085,#4086,#4087));
#1071=EDGE_LOOP('',(#4088,#4089,#4090,#4091));
#1072=EDGE_LOOP('',(#4092));
#1073=EDGE_LOOP('',(#4093));
#1074=EDGE_LOOP('',(#4094,#4095,#4096,#4097,#4098));
#1075=EDGE_LOOP('',(#4099,#4100));
#1076=EDGE_LOOP('',(#4101,#4102));
#1077=EDGE_LOOP('',(#4103,#4104));
#1078=EDGE_LOOP('',(#4105,#4106));
#1079=EDGE_LOOP('',(#4107,#4108));
#1080=EDGE_LOOP('',(#4109,#4110));
#1081=EDGE_LOOP('',(#4111,#4112));
#1082=EDGE_LOOP('',(#4113,#4114));
#1083=EDGE_LOOP('',(#4115,#4116,#4117,#4118));
#1084=EDGE_LOOP('',(#4119,#4120,#4121,#4122,#4123,#4124,#4125,#4126,#4127,
#4128,#4129,#4130,#4131,#4132,#4133,#4134,#4135,#4136,#4137,#4138));
#1085=EDGE_LOOP('',(#4139,#4140,#4141,#4142));
#1086=EDGE_LOOP('',(#4143,#4144,#4145,#4146));
#1087=EDGE_LOOP('',(#4147,#4148,#4149,#4150));
#1088=EDGE_LOOP('',(#4151,#4152,#4153,#4154));
#1089=EDGE_LOOP('',(#4155,#4156,#4157,#4158));
#1090=EDGE_LOOP('',(#4159,#4160,#4161,#4162,#4163,#4164));
#1091=EDGE_LOOP('',(#4165,#4166,#4167,#4168));
#1092=EDGE_LOOP('',(#4169,#4170,#4171,#4172));
#1093=EDGE_LOOP('',(#4173,#4174,#4175,#4176));
#1094=EDGE_LOOP('',(#4177,#4178,#4179,#4180));
#1095=EDGE_LOOP('',(#4181,#4182,#4183,#4184));
#1096=EDGE_LOOP('',(#4185,#4186,#4187,#4188));
#1097=EDGE_LOOP('',(#4189,#4190,#4191,#4192,#4193,#4194,#4195,#4196,#4197,
#4198,#4199,#4200,#4201,#4202,#4203,#4204,#4205,#4206,#4207,#4208));
#1098=EDGE_LOOP('',(#4209,#4210,#4211,#4212));
#1099=EDGE_LOOP('',(#4213,#4214,#4215,#4216));
#1100=EDGE_LOOP('',(#4217));
#1101=EDGE_LOOP('',(#4218));
#1102=EDGE_LOOP('',(#4219,#4220,#4221,#4222));
#1103=EDGE_LOOP('',(#4223));
#1104=EDGE_LOOP('',(#4224));
#1105=EDGE_LOOP('',(#4225,#4226,#4227,#4228));
#1106=EDGE_LOOP('',(#4229));
#1107=EDGE_LOOP('',(#4230));
#1108=EDGE_LOOP('',(#4231,#4232,#4233,#4234));
#1109=EDGE_LOOP('',(#4235));
#1110=EDGE_LOOP('',(#4236));
#1111=EDGE_LOOP('',(#4237,#4238,#4239,#4240));
#1112=EDGE_LOOP('',(#4241));
#1113=EDGE_LOOP('',(#4242));
#1114=EDGE_LOOP('',(#4243,#4244,#4245,#4246));
#1115=EDGE_LOOP('',(#4247));
#1116=EDGE_LOOP('',(#4248,#4249,#4250,#4251));
#1117=EDGE_LOOP('',(#4252,#4253,#4254,#4255));
#1118=EDGE_LOOP('',(#4256,#4257,#4258,#4259));
#1119=EDGE_LOOP('',(#4260));
#1120=EDGE_LOOP('',(#4261));
#1121=EDGE_LOOP('',(#4262,#4263,#4264,#4265));
#1122=EDGE_LOOP('',(#4266,#4267,#4268,#4269));
#1123=EDGE_LOOP('',(#4270,#4271,#4272,#4273));
#1124=EDGE_LOOP('',(#4274));
#1125=EDGE_LOOP('',(#4275,#4276,#4277,#4278));
#1126=EDGE_LOOP('',(#4279,#4280,#4281,#4282));
#1127=EDGE_LOOP('',(#4283,#4284,#4285,#4286));
#1128=EDGE_LOOP('',(#4287,#4288,#4289,#4290));
#1129=EDGE_LOOP('',(#4291,#4292,#4293,#4294));
#1130=EDGE_LOOP('',(#4295,#4296,#4297,#4298));
#1131=EDGE_LOOP('',(#4299,#4300,#4301,#4302,#4303,#4304));
#1132=EDGE_LOOP('',(#4305,#4306,#4307,#4308,#4309,#4310));
#1133=EDGE_LOOP('',(#4311));
#1134=EDGE_LOOP('',(#4312,#4313,#4314,#4315));
#1135=EDGE_LOOP('',(#4316,#4317,#4318,#4319));
#1136=EDGE_LOOP('',(#4320,#4321,#4322,#4323));
#1137=EDGE_LOOP('',(#4324));
#1138=EDGE_LOOP('',(#4325));
#1139=EDGE_LOOP('',(#4326,#4327,#4328,#4329));
#1140=EDGE_LOOP('',(#4330,#4331,#4332,#4333));
#1141=EDGE_LOOP('',(#4334,#4335,#4336,#4337));
#1142=EDGE_LOOP('',(#4338));
#1143=EDGE_LOOP('',(#4339,#4340,#4341,#4342));
#1144=EDGE_LOOP('',(#4343,#4344,#4345,#4346));
#1145=EDGE_LOOP('',(#4347,#4348,#4349,#4350));
#1146=EDGE_LOOP('',(#4351,#4352,#4353,#4354));
#1147=EDGE_LOOP('',(#4355,#4356,#4357,#4358));
#1148=EDGE_LOOP('',(#4359,#4360,#4361,#4362));
#1149=EDGE_LOOP('',(#4363,#4364,#4365,#4366,#4367,#4368));
#1150=EDGE_LOOP('',(#4369,#4370,#4371,#4372,#4373,#4374));
#1151=EDGE_LOOP('',(#4375,#4376,#4377,#4378));
#1152=EDGE_LOOP('',(#4379,#4380,#4381,#4382));
#1153=EDGE_LOOP('',(#4383,#4384,#4385,#4386));
#1154=EDGE_LOOP('',(#4387,#4388,#4389,#4390));
#1155=EDGE_LOOP('',(#4391,#4392,#4393,#4394));
#1156=EDGE_LOOP('',(#4395,#4396,#4397,#4398));
#1157=EDGE_LOOP('',(#4399,#4400,#4401,#4402));
#1158=EDGE_LOOP('',(#4403));
#1159=EDGE_LOOP('',(#4404));
#1160=EDGE_LOOP('',(#4405));
#1161=EDGE_LOOP('',(#4406));
#1162=EDGE_LOOP('',(#4407));
#1163=EDGE_LOOP('',(#4408,#4409,#4410,#4411));
#1164=EDGE_LOOP('',(#4412,#4413,#4414,#4415));
#1165=EDGE_LOOP('',(#4416,#4417,#4418,#4419));
#1166=EDGE_LOOP('',(#4420));
#1167=EDGE_LOOP('',(#4421));
#1168=EDGE_LOOP('',(#4422));
#1169=EDGE_LOOP('',(#4423,#4424,#4425,#4426));
#1170=EDGE_LOOP('',(#4427,#4428,#4429,#4430));
#1171=EDGE_LOOP('',(#4431));
#1172=EDGE_LOOP('',(#4432));
#1173=EDGE_LOOP('',(#4433));
#1174=EDGE_LOOP('',(#4434));
#1175=EDGE_LOOP('',(#4435,#4436));
#1176=EDGE_LOOP('',(#4437,#4438,#4439,#4440,#4441,#4442,#4443,#4444,#4445));
#1177=EDGE_LOOP('',(#4446,#4447,#4448));
#1178=EDGE_LOOP('',(#4449,#4450,#4451,#4452));
#1179=EDGE_LOOP('',(#4453,#4454,#4455,#4456));
#1180=EDGE_LOOP('',(#4457,#4458,#4459,#4460));
#1181=EDGE_LOOP('',(#4461,#4462));
#1182=EDGE_LOOP('',(#4463));
#1183=EDGE_LOOP('',(#4464));
#1184=EDGE_LOOP('',(#4465));
#1185=EDGE_LOOP('',(#4466));
#1186=EDGE_LOOP('',(#4467,#4468));
#1187=EDGE_LOOP('',(#4469,#4470,#4471,#4472,#4473,#4474,#4475,#4476,#4477));
#1188=EDGE_LOOP('',(#4478,#4479,#4480));
#1189=EDGE_LOOP('',(#4481,#4482,#4483,#4484));
#1190=EDGE_LOOP('',(#4485,#4486,#4487,#4488));
#1191=EDGE_LOOP('',(#4489,#4490,#4491,#4492));
#1192=EDGE_LOOP('',(#4493,#4494));
#1193=EDGE_LOOP('',(#4495));
#1194=EDGE_LOOP('',(#4496));
#1195=EDGE_LOOP('',(#4497));
#1196=EDGE_LOOP('',(#4498));
#1197=EDGE_LOOP('',(#4499,#4500,#4501,#4502));
#1198=EDGE_LOOP('',(#4503,#4504,#4505,#4506));
#1199=EDGE_LOOP('',(#4507));
#1200=EDGE_LOOP('',(#4508,#4509,#4510,#4511));
#1201=EDGE_LOOP('',(#4512));
#1202=EDGE_LOOP('',(#4513,#4514,#4515,#4516));
#1203=EDGE_LOOP('',(#4517,#4518,#4519,#4520));
#1204=EDGE_LOOP('',(#4521,#4522));
#1205=EDGE_LOOP('',(#4523,#4524));
#1206=EDGE_LOOP('',(#4525,#4526));
#1207=EDGE_LOOP('',(#4527,#4528,#4529,#4530,#4531,#4532,#4533));
#1208=EDGE_LOOP('',(#4534,#4535,#4536,#4537,#4538,#4539,#4540));
#1209=EDGE_LOOP('',(#4541,#4542,#4543,#4544,#4545,#4546,#4547,#4548,#4549));
#1210=EDGE_LOOP('',(#4550,#4551,#4552));
#1211=EDGE_LOOP('',(#4553,#4554,#4555));
#1212=EDGE_LOOP('',(#4556,#4557,#4558));
#1213=EDGE_LOOP('',(#4559,#4560,#4561,#4562,#4563,#4564));
#1214=EDGE_LOOP('',(#4565,#4566,#4567,#4568,#4569,#4570,#4571));
#1215=EDGE_LOOP('',(#4572));
#1216=EDGE_LOOP('',(#4573,#4574,#4575,#4576));
#1217=EDGE_LOOP('',(#4577));
#1218=EDGE_LOOP('',(#4578,#4579,#4580,#4581,#4582,#4583,#4584,#4585,#4586,
#4587,#4588,#4589,#4590,#4591,#4592,#4593,#4594,#4595,#4596,#4597,#4598,
#4599,#4600,#4601,#4602,#4603,#4604,#4605,#4606,#4607,#4608,#4609,#4610,
#4611,#4612,#4613,#4614,#4615,#4616,#4617,#4618,#4619,#4620,#4621,#4622,
#4623,#4624,#4625,#4626,#4627,#4628,#4629,#4630,#4631,#4632,#4633,#4634,
#4635,#4636,#4637,#4638,#4639,#4640,#4641,#4642,#4643,#4644,#4645,#4646,
#4647,#4648,#4649,#4650,#4651,#4652,#4653,#4654,#4655,#4656,#4657));
#1219=EDGE_LOOP('',(#4658,#4659,#4660,#4661));
#1220=EDGE_LOOP('',(#4662));
#1221=EDGE_LOOP('',(#4663));
#1222=EDGE_LOOP('',(#4664));
#1223=EDGE_LOOP('',(#4665,#4666,#4667,#4668,#4669,#4670,#4671,#4672,#4673,
#4674,#4675,#4676,#4677,#4678,#4679,#4680,#4681,#4682,#4683,#4684,#4685,
#4686,#4687,#4688,#4689,#4690,#4691,#4692,#4693,#4694,#4695,#4696,#4697,
#4698,#4699,#4700,#4701,#4702,#4703,#4704,#4705,#4706,#4707,#4708,#4709,
#4710,#4711,#4712,#4713,#4714,#4715,#4716,#4717,#4718,#4719,#4720,#4721,
#4722,#4723,#4724,#4725,#4726,#4727,#4728,#4729,#4730,#4731,#4732,#4733,
#4734,#4735,#4736,#4737,#4738,#4739,#4740,#4741,#4742,#4743,#4744));
#1224=EDGE_LOOP('',(#4745,#4746,#4747,#4748));
#1225=EDGE_LOOP('',(#4749,#4750,#4751,#4752));
#1226=EDGE_LOOP('',(#4753,#4754,#4755,#4756));
#1227=EDGE_LOOP('',(#4757,#4758,#4759,#4760));
#1228=EDGE_LOOP('',(#4761,#4762,#4763,#4764));
#1229=EDGE_LOOP('',(#4765,#4766,#4767,#4768));
#1230=EDGE_LOOP('',(#4769,#4770,#4771,#4772));
#1231=EDGE_LOOP('',(#4773,#4774,#4775,#4776));
#1232=EDGE_LOOP('',(#4777,#4778,#4779,#4780));
#1233=EDGE_LOOP('',(#4781,#4782,#4783,#4784));
#1234=EDGE_LOOP('',(#4785,#4786,#4787,#4788));
#1235=EDGE_LOOP('',(#4789,#4790,#4791,#4792));
#1236=EDGE_LOOP('',(#4793,#4794,#4795,#4796));
#1237=EDGE_LOOP('',(#4797,#4798,#4799,#4800));
#1238=EDGE_LOOP('',(#4801,#4802,#4803,#4804));
#1239=EDGE_LOOP('',(#4805,#4806,#4807,#4808));
#1240=EDGE_LOOP('',(#4809,#4810,#4811,#4812));
#1241=EDGE_LOOP('',(#4813,#4814,#4815,#4816));
#1242=EDGE_LOOP('',(#4817,#4818,#4819,#4820));
#1243=EDGE_LOOP('',(#4821,#4822,#4823,#4824));
#1244=EDGE_LOOP('',(#4825,#4826,#4827,#4828));
#1245=EDGE_LOOP('',(#4829,#4830,#4831,#4832));
#1246=EDGE_LOOP('',(#4833,#4834,#4835,#4836));
#1247=EDGE_LOOP('',(#4837,#4838,#4839,#4840));
#1248=EDGE_LOOP('',(#4841,#4842,#4843,#4844));
#1249=EDGE_LOOP('',(#4845,#4846,#4847,#4848));
#1250=EDGE_LOOP('',(#4849,#4850,#4851,#4852));
#1251=EDGE_LOOP('',(#4853,#4854,#4855,#4856));
#1252=EDGE_LOOP('',(#4857,#4858,#4859,#4860));
#1253=EDGE_LOOP('',(#4861,#4862,#4863,#4864));
#1254=EDGE_LOOP('',(#4865,#4866,#4867,#4868));
#1255=EDGE_LOOP('',(#4869,#4870,#4871,#4872));
#1256=EDGE_LOOP('',(#4873,#4874,#4875,#4876));
#1257=EDGE_LOOP('',(#4877,#4878,#4879,#4880));
#1258=EDGE_LOOP('',(#4881,#4882,#4883,#4884));
#1259=EDGE_LOOP('',(#4885,#4886,#4887,#4888));
#1260=EDGE_LOOP('',(#4889,#4890,#4891,#4892));
#1261=EDGE_LOOP('',(#4893,#4894,#4895,#4896));
#1262=EDGE_LOOP('',(#4897,#4898,#4899,#4900));
#1263=EDGE_LOOP('',(#4901,#4902,#4903,#4904));
#1264=EDGE_LOOP('',(#4905,#4906,#4907,#4908));
#1265=EDGE_LOOP('',(#4909,#4910,#4911,#4912));
#1266=EDGE_LOOP('',(#4913,#4914,#4915,#4916));
#1267=EDGE_LOOP('',(#4917,#4918,#4919,#4920));
#1268=EDGE_LOOP('',(#4921,#4922,#4923,#4924));
#1269=EDGE_LOOP('',(#4925,#4926,#4927,#4928));
#1270=EDGE_LOOP('',(#4929,#4930,#4931,#4932));
#1271=EDGE_LOOP('',(#4933,#4934,#4935,#4936));
#1272=EDGE_LOOP('',(#4937,#4938,#4939,#4940));
#1273=EDGE_LOOP('',(#4941,#4942,#4943,#4944));
#1274=EDGE_LOOP('',(#4945,#4946,#4947,#4948));
#1275=EDGE_LOOP('',(#4949,#4950,#4951,#4952));
#1276=EDGE_LOOP('',(#4953,#4954,#4955,#4956));
#1277=EDGE_LOOP('',(#4957,#4958,#4959,#4960));
#1278=EDGE_LOOP('',(#4961,#4962,#4963,#4964));
#1279=EDGE_LOOP('',(#4965,#4966,#4967,#4968));
#1280=EDGE_LOOP('',(#4969,#4970,#4971,#4972));
#1281=EDGE_LOOP('',(#4973,#4974,#4975,#4976));
#1282=EDGE_LOOP('',(#4977,#4978,#4979,#4980));
#1283=EDGE_LOOP('',(#4981,#4982,#4983,#4984));
#1284=EDGE_LOOP('',(#4985,#4986,#4987,#4988));
#1285=EDGE_LOOP('',(#4989,#4990,#4991,#4992));
#1286=EDGE_LOOP('',(#4993,#4994,#4995,#4996));
#1287=EDGE_LOOP('',(#4997,#4998,#4999,#5000));
#1288=EDGE_LOOP('',(#5001,#5002,#5003,#5004));
#1289=EDGE_LOOP('',(#5005,#5006,#5007,#5008));
#1290=EDGE_LOOP('',(#5009,#5010,#5011,#5012));
#1291=EDGE_LOOP('',(#5013,#5014,#5015,#5016));
#1292=EDGE_LOOP('',(#5017,#5018,#5019,#5020));
#1293=EDGE_LOOP('',(#5021,#5022,#5023,#5024));
#1294=EDGE_LOOP('',(#5025,#5026,#5027,#5028));
#1295=EDGE_LOOP('',(#5029,#5030,#5031,#5032));
#1296=EDGE_LOOP('',(#5033,#5034,#5035,#5036));
#1297=EDGE_LOOP('',(#5037,#5038,#5039,#5040));
#1298=EDGE_LOOP('',(#5041,#5042,#5043,#5044));
#1299=EDGE_LOOP('',(#5045,#5046,#5047,#5048));
#1300=EDGE_LOOP('',(#5049,#5050,#5051,#5052));
#1301=EDGE_LOOP('',(#5053,#5054,#5055,#5056));
#1302=EDGE_LOOP('',(#5057,#5058,#5059,#5060));
#1303=EDGE_LOOP('',(#5061,#5062,#5063,#5064));
#1304=EDGE_LOOP('',(#5065,#5066,#5067,#5068));
#1305=EDGE_LOOP('',(#5069,#5070,#5071,#5072,#5073,#5074,#5075,#5076));
#1306=EDGE_LOOP('',(#5077,#5078,#5079,#5080));
#1307=EDGE_LOOP('',(#5081,#5082,#5083,#5084));
#1308=EDGE_LOOP('',(#5085,#5086,#5087,#5088));
#1309=EDGE_LOOP('',(#5089,#5090,#5091,#5092));
#1310=EDGE_LOOP('',(#5093,#5094,#5095,#5096,#5097,#5098,#5099,#5100));
#1311=EDGE_LOOP('',(#5101,#5102,#5103,#5104));
#1312=EDGE_LOOP('',(#5105,#5106,#5107,#5108));
#1313=EDGE_LOOP('',(#5109,#5110,#5111,#5112));
#1314=EDGE_LOOP('',(#5113,#5114,#5115,#5116));
#1315=EDGE_LOOP('',(#5117,#5118,#5119,#5120));
#1316=EDGE_LOOP('',(#5121,#5122,#5123,#5124));
#1317=EDGE_LOOP('',(#5125,#5126,#5127,#5128));
#1318=EDGE_LOOP('',(#5129,#5130,#5131,#5132));
#1319=EDGE_LOOP('',(#5133,#5134,#5135,#5136));
#1320=EDGE_LOOP('',(#5137,#5138,#5139,#5140));
#1321=EDGE_LOOP('',(#5141,#5142,#5143,#5144,#5145,#5146));
#1322=EDGE_LOOP('',(#5147));
#1323=EDGE_LOOP('',(#5148,#5149,#5150,#5151,#5152,#5153));
#1324=EDGE_LOOP('',(#5154,#5155,#5156,#5157));
#1325=EDGE_LOOP('',(#5158,#5159,#5160,#5161));
#1326=EDGE_LOOP('',(#5162,#5163,#5164,#5165));
#1327=EDGE_LOOP('',(#5166));
#1328=LINE('',#8563,#1670);
#1329=LINE('',#8569,#1671);
#1330=LINE('',#8575,#1672);
#1331=LINE('',#8581,#1673);
#1332=LINE('',#8586,#1674);
#1333=LINE('',#8588,#1675);
#1334=LINE('',#8590,#1676);
#1335=LINE('',#8591,#1677);
#1336=LINE('',#8594,#1678);
#1337=LINE('',#8596,#1679);
#1338=LINE('',#8597,#1680);
#1339=LINE('',#8600,#1681);
#1340=LINE('',#8602,#1682);
#1341=LINE('',#8603,#1683);
#1342=LINE('',#8605,#1684);
#1343=LINE('',#8606,#1685);
#1344=LINE('',#8614,#1686);
#1345=LINE('',#8621,#1687);
#1346=LINE('',#8628,#1688);
#1347=LINE('',#8635,#1689);
#1348=LINE('',#8642,#1690);
#1349=LINE('',#8649,#1691);
#1350=LINE('',#8656,#1692);
#1351=LINE('',#8663,#1693);
#1352=LINE('',#8670,#1694);
#1353=LINE('',#8676,#1695);
#1354=LINE('',#8682,#1696);
#1355=LINE('',#8688,#1697);
#1356=LINE('',#8695,#1698);
#1357=LINE('',#8697,#1699);
#1358=LINE('',#8698,#1700);
#1359=LINE('',#8703,#1701);
#1360=LINE('',#8705,#1702);
#1361=LINE('',#8706,#1703);
#1362=LINE('',#8712,#1704);
#1363=LINE('',#8714,#1705);
#1364=LINE('',#8715,#1706);
#1365=LINE('',#8720,#1707);
#1366=LINE('',#8722,#1708);
#1367=LINE('',#8723,#1709);
#1368=LINE('',#8725,#1710);
#1369=LINE('',#8726,#1711);
#1370=LINE('',#8728,#1712);
#1371=LINE('',#8729,#1713);
#1372=LINE('',#8731,#1714);
#1373=LINE('',#8733,#1715);
#1374=LINE('',#8740,#1716);
#1375=LINE('',#8742,#1717);
#1376=LINE('',#8743,#1718);
#1377=LINE('',#8748,#1719);
#1378=LINE('',#8750,#1720);
#1379=LINE('',#8751,#1721);
#1380=LINE('',#8757,#1722);
#1381=LINE('',#8759,#1723);
#1382=LINE('',#8760,#1724);
#1383=LINE('',#8765,#1725);
#1384=LINE('',#8767,#1726);
#1385=LINE('',#8768,#1727);
#1386=LINE('',#8770,#1728);
#1387=LINE('',#8771,#1729);
#1388=LINE('',#8773,#1730);
#1389=LINE('',#8774,#1731);
#1390=LINE('',#8776,#1732);
#1391=LINE('',#8778,#1733);
#1392=LINE('',#8784,#1734);
#1393=LINE('',#8790,#1735);
#1394=LINE('',#8799,#1736);
#1395=LINE('',#8805,#1737);
#1396=LINE('',#8814,#1738);
#1397=LINE('',#8820,#1739);
#1398=LINE('',#8826,#1740);
#1399=LINE('',#8832,#1741);
#1400=LINE('',#8838,#1742);
#1401=LINE('',#8847,#1743);
#1402=LINE('',#8853,#1744);
#1403=LINE('',#8858,#1745);
#1404=LINE('',#8867,#1746);
#1405=LINE('',#8873,#1747);
#1406=LINE('',#8882,#1748);
#1407=LINE('',#8888,#1749);
#1408=LINE('',#8894,#1750);
#1409=LINE('',#8900,#1751);
#1410=LINE('',#8906,#1752);
#1411=LINE('',#8914,#1753);
#1412=LINE('',#8919,#1754);
#1413=LINE('',#8927,#1755);
#1414=LINE('',#8929,#1756);
#1415=LINE('',#8931,#1757);
#1416=LINE('',#8932,#1758);
#1417=LINE('',#8935,#1759);
#1418=LINE('',#8937,#1760);
#1419=LINE('',#8938,#1761);
#1420=LINE('',#8941,#1762);
#1421=LINE('',#8943,#1763);
#1422=LINE('',#8944,#1764);
#1423=LINE('',#8946,#1765);
#1424=LINE('',#8947,#1766);
#1425=LINE('',#8954,#1767);
#1426=LINE('',#8956,#1768);
#1427=LINE('',#8958,#1769);
#1428=LINE('',#8959,#1770);
#1429=LINE('',#8962,#1771);
#1430=LINE('',#8964,#1772);
#1431=LINE('',#8965,#1773);
#1432=LINE('',#8968,#1774);
#1433=LINE('',#8970,#1775);
#1434=LINE('',#8971,#1776);
#1435=LINE('',#8973,#1777);
#1436=LINE('',#8974,#1778);
#1437=LINE('',#8991,#1779);
#1438=LINE('',#8997,#1780);
#1439=LINE('',#9001,#1781);
#1440=LINE('',#9007,#1782);
#1441=LINE('',#9012,#1783);
#1442=LINE('',#9027,#1784);
#1443=LINE('',#9036,#1785);
#1444=LINE('',#9040,#1786);
#1445=LINE('',#9044,#1787);
#1446=LINE('',#9047,#1788);
#1447=LINE('',#9200,#1789);
#1448=LINE('',#9496,#1790);
#1449=LINE('',#9538,#1791);
#1450=LINE('',#9543,#1792);
#1451=LINE('',#9552,#1793);
#1452=LINE('',#9557,#1794);
#1453=LINE('',#9570,#1795);
#1454=LINE('',#9574,#1796);
#1455=LINE('',#9578,#1797);
#1456=LINE('',#9585,#1798);
#1457=LINE('',#9589,#1799);
#1458=LINE('',#9593,#1800);
#1459=LINE('',#9598,#1801);
#1460=LINE('',#9600,#1802);
#1461=LINE('',#9602,#1803);
#1462=LINE('',#9603,#1804);
#1463=LINE('',#9606,#1805);
#1464=LINE('',#9608,#1806);
#1465=LINE('',#9609,#1807);
#1466=LINE('',#9612,#1808);
#1467=LINE('',#9614,#1809);
#1468=LINE('',#9615,#1810);
#1469=LINE('',#9618,#1811);
#1470=LINE('',#9620,#1812);
#1471=LINE('',#9621,#1813);
#1472=LINE('',#9624,#1814);
#1473=LINE('',#9626,#1815);
#1474=LINE('',#9627,#1816);
#1475=LINE('',#9629,#1817);
#1476=LINE('',#9630,#1818);
#1477=LINE('',#9640,#1819);
#1478=LINE('',#9644,#1820);
#1479=LINE('',#9648,#1821);
#1480=LINE('',#9655,#1822);
#1481=LINE('',#9659,#1823);
#1482=LINE('',#9663,#1824);
#1483=LINE('',#9668,#1825);
#1484=LINE('',#9670,#1826);
#1485=LINE('',#9672,#1827);
#1486=LINE('',#9673,#1828);
#1487=LINE('',#9676,#1829);
#1488=LINE('',#9678,#1830);
#1489=LINE('',#9679,#1831);
#1490=LINE('',#9682,#1832);
#1491=LINE('',#9684,#1833);
#1492=LINE('',#9685,#1834);
#1493=LINE('',#9688,#1835);
#1494=LINE('',#9690,#1836);
#1495=LINE('',#9691,#1837);
#1496=LINE('',#9694,#1838);
#1497=LINE('',#9696,#1839);
#1498=LINE('',#9697,#1840);
#1499=LINE('',#9699,#1841);
#1500=LINE('',#9700,#1842);
#1501=LINE('',#9730,#1843);
#1502=LINE('',#9732,#1844);
#1503=LINE('',#9734,#1845);
#1504=LINE('',#9735,#1846);
#1505=LINE('',#9740,#1847);
#1506=LINE('',#9741,#1848);
#1507=LINE('',#9744,#1849);
#1508=LINE('',#9746,#1850);
#1509=LINE('',#9747,#1851);
#1510=LINE('',#9749,#1852);
#1511=LINE('',#9756,#1853);
#1512=LINE('',#9770,#1854);
#1513=LINE('',#9773,#1855);
#1514=LINE('',#9778,#1856);
#1515=LINE('',#9786,#1857);
#1516=LINE('',#9792,#1858);
#1517=LINE('',#9800,#1859);
#1518=LINE('',#9821,#1860);
#1519=LINE('',#9876,#1861);
#1520=LINE('',#9881,#1862);
#1521=LINE('',#9887,#1863);
#1522=LINE('',#9895,#1864);
#1523=LINE('',#9912,#1865);
#1524=LINE('',#9963,#1866);
#1525=LINE('',#9968,#1867);
#1526=LINE('',#9974,#1868);
#1527=LINE('',#9982,#1869);
#1528=LINE('',#9984,#1870);
#1529=LINE('',#9986,#1871);
#1530=LINE('',#9987,#1872);
#1531=LINE('',#9990,#1873);
#1532=LINE('',#9992,#1874);
#1533=LINE('',#9993,#1875);
#1534=LINE('',#9998,#1876);
#1535=LINE('',#10000,#1877);
#1536=LINE('',#10001,#1878);
#1537=LINE('',#10164,#1879);
#1538=LINE('',#10167,#1880);
#1539=LINE('',#10211,#1881);
#1540=LINE('',#10213,#1882);
#1541=LINE('',#10298,#1883);
#1542=LINE('',#10300,#1884);
#1543=LINE('',#10468,#1885);
#1544=LINE('',#10634,#1886);
#1545=LINE('',#10636,#1887);
#1546=LINE('',#10637,#1888);
#1547=LINE('',#10639,#1889);
#1548=LINE('',#10641,#1890);
#1549=LINE('',#10643,#1891);
#1550=LINE('',#10645,#1892);
#1551=LINE('',#10647,#1893);
#1552=LINE('',#10649,#1894);
#1553=LINE('',#10651,#1895);
#1554=LINE('',#10653,#1896);
#1555=LINE('',#10655,#1897);
#1556=LINE('',#10657,#1898);
#1557=LINE('',#10659,#1899);
#1558=LINE('',#10661,#1900);
#1559=LINE('',#10663,#1901);
#1560=LINE('',#10665,#1902);
#1561=LINE('',#10667,#1903);
#1562=LINE('',#10669,#1904);
#1563=LINE('',#10671,#1905);
#1564=LINE('',#10673,#1906);
#1565=LINE('',#10675,#1907);
#1566=LINE('',#10677,#1908);
#1567=LINE('',#10679,#1909);
#1568=LINE('',#10681,#1910);
#1569=LINE('',#10683,#1911);
#1570=LINE('',#10685,#1912);
#1571=LINE('',#10687,#1913);
#1572=LINE('',#10689,#1914);
#1573=LINE('',#10691,#1915);
#1574=LINE('',#10693,#1916);
#1575=LINE('',#10695,#1917);
#1576=LINE('',#10697,#1918);
#1577=LINE('',#10699,#1919);
#1578=LINE('',#10701,#1920);
#1579=LINE('',#10703,#1921);
#1580=LINE('',#10705,#1922);
#1581=LINE('',#10707,#1923);
#1582=LINE('',#10709,#1924);
#1583=LINE('',#10711,#1925);
#1584=LINE('',#10713,#1926);
#1585=LINE('',#10715,#1927);
#1586=LINE('',#10717,#1928);
#1587=LINE('',#10719,#1929);
#1588=LINE('',#10721,#1930);
#1589=LINE('',#10723,#1931);
#1590=LINE('',#10725,#1932);
#1591=LINE('',#10727,#1933);
#1592=LINE('',#10729,#1934);
#1593=LINE('',#10731,#1935);
#1594=LINE('',#10733,#1936);
#1595=LINE('',#10735,#1937);
#1596=LINE('',#10737,#1938);
#1597=LINE('',#10739,#1939);
#1598=LINE('',#10741,#1940);
#1599=LINE('',#10743,#1941);
#1600=LINE('',#10745,#1942);
#1601=LINE('',#10747,#1943);
#1602=LINE('',#10749,#1944);
#1603=LINE('',#10751,#1945);
#1604=LINE('',#10753,#1946);
#1605=LINE('',#10755,#1947);
#1606=LINE('',#10757,#1948);
#1607=LINE('',#10759,#1949);
#1608=LINE('',#10761,#1950);
#1609=LINE('',#10763,#1951);
#1610=LINE('',#10765,#1952);
#1611=LINE('',#10767,#1953);
#1612=LINE('',#10769,#1954);
#1613=LINE('',#10771,#1955);
#1614=LINE('',#10773,#1956);
#1615=LINE('',#10775,#1957);
#1616=LINE('',#10777,#1958);
#1617=LINE('',#10779,#1959);
#1618=LINE('',#10781,#1960);
#1619=LINE('',#10783,#1961);
#1620=LINE('',#10785,#1962);
#1621=LINE('',#10787,#1963);
#1622=LINE('',#10789,#1964);
#1623=LINE('',#10791,#1965);
#1624=LINE('',#10793,#1966);
#1625=LINE('',#10799,#1967);
#1626=LINE('',#10801,#1968);
#1627=LINE('',#10803,#1969);
#1628=LINE('',#10805,#1970);
#1629=LINE('',#10807,#1971);
#1630=LINE('',#10809,#1972);
#1631=LINE('',#10811,#1973);
#1632=LINE('',#10812,#1974);
#1633=LINE('',#10815,#1975);
#1634=LINE('',#10817,#1976);
#1635=LINE('',#10818,#1977);
#1636=LINE('',#10821,#1978);
#1637=LINE('',#10822,#1979);
#1638=LINE('',#10825,#1980);
#1639=LINE('',#10826,#1981);
#1640=LINE('',#10829,#1982);
#1641=LINE('',#10830,#1983);
#1642=LINE('',#10833,#1984);
#1643=LINE('',#10835,#1985);
#1644=LINE('',#10837,#1986);
#1645=LINE('',#10838,#1987);
#1646=LINE('',#10840,#1988);
#1647=LINE('',#10842,#1989);
#1648=LINE('',#10844,#1990);
#1649=LINE('',#10850,#1991);
#1650=LINE('',#10852,#1992);
#1651=LINE('',#10854,#1993);
#1652=LINE('',#10855,#1994);
#1653=LINE('',#10858,#1995);
#1654=LINE('',#10860,#1996);
#1655=LINE('',#10861,#1997);
#1656=LINE('',#10864,#1998);
#1657=LINE('',#10866,#1999);
#1658=LINE('',#10867,#2000);
#1659=LINE('',#10870,#2001);
#1660=LINE('',#10872,#2002);
#1661=LINE('',#10873,#2003);
#1662=LINE('',#10876,#2004);
#1663=LINE('',#10878,#2005);
#1664=LINE('',#10879,#2006);
#1665=LINE('',#10881,#2007);
#1666=LINE('',#10882,#2008);
#1667=LINE('',#10890,#2009);
#1668=LINE('',#10894,#2010);
#1669=LINE('',#10898,#2011);
#1670=VECTOR('',#6698,0.25);
#1671=VECTOR('',#6705,0.25);
#1672=VECTOR('',#6712,0.25);
#1673=VECTOR('',#6719,0.25);
#1674=VECTOR('',#6724,1.);
#1675=VECTOR('',#6725,1.);
#1676=VECTOR('',#6726,1.);
#1677=VECTOR('',#6727,1.);
#1678=VECTOR('',#6730,1.);
#1679=VECTOR('',#6731,1.);
#1680=VECTOR('',#6732,1.);
#1681=VECTOR('',#6735,1.);
#1682=VECTOR('',#6736,1.);
#1683=VECTOR('',#6737,1.);
#1684=VECTOR('',#6740,1.);
#1685=VECTOR('',#6741,1.);
#1686=VECTOR('',#6752,0.165);
#1687=VECTOR('',#6761,0.165);
#1688=VECTOR('',#6770,0.165);
#1689=VECTOR('',#6779,0.165);
#1690=VECTOR('',#6788,0.165);
#1691=VECTOR('',#6797,0.165);
#1692=VECTOR('',#6806,0.165);
#1693=VECTOR('',#6815,0.165);
#1694=VECTOR('',#6824,0.33);
#1695=VECTOR('',#6831,0.33);
#1696=VECTOR('',#6838,0.33);
#1697=VECTOR('',#6845,0.33);
#1698=VECTOR('',#6852,1.);
#1699=VECTOR('',#6853,1.);
#1700=VECTOR('',#6854,1.);
#1701=VECTOR('',#6859,1.);
#1702=VECTOR('',#6860,1.);
#1703=VECTOR('',#6861,1.);
#1704=VECTOR('',#6866,1.);
#1705=VECTOR('',#6867,1.);
#1706=VECTOR('',#6868,1.);
#1707=VECTOR('',#6873,1.);
#1708=VECTOR('',#6874,1.);
#1709=VECTOR('',#6875,1.);
#1710=VECTOR('',#6878,1.);
#1711=VECTOR('',#6879,1.);
#1712=VECTOR('',#6882,1.);
#1713=VECTOR('',#6883,1.);
#1714=VECTOR('',#6886,1.);
#1715=VECTOR('',#6889,1.);
#1716=VECTOR('',#6896,1.);
#1717=VECTOR('',#6897,1.);
#1718=VECTOR('',#6898,1.);
#1719=VECTOR('',#6903,1.);
#1720=VECTOR('',#6904,1.);
#1721=VECTOR('',#6905,1.);
#1722=VECTOR('',#6910,1.);
#1723=VECTOR('',#6911,1.);
#1724=VECTOR('',#6912,1.);
#1725=VECTOR('',#6917,1.);
#1726=VECTOR('',#6918,1.);
#1727=VECTOR('',#6919,1.);
#1728=VECTOR('',#6922,1.);
#1729=VECTOR('',#6923,1.);
#1730=VECTOR('',#6926,1.);
#1731=VECTOR('',#6927,1.);
#1732=VECTOR('',#6930,1.);
#1733=VECTOR('',#6933,1.);
#1734=VECTOR('',#6940,2.35);
#1735=VECTOR('',#6947,3.5);
#1736=VECTOR('',#6960,1.75);
#1737=VECTOR('',#6967,2.34);
#1738=VECTOR('',#6980,0.225);
#1739=VECTOR('',#6987,0.225);
#1740=VECTOR('',#6994,0.225);
#1741=VECTOR('',#7001,0.225);
#1742=VECTOR('',#7008,2.34);
#1743=VECTOR('',#7019,1.8);
#1744=VECTOR('',#7028,1.6);
#1745=VECTOR('',#7033,3.5);
#1746=VECTOR('',#7046,1.);
#1747=VECTOR('',#7053,1.8);
#1748=VECTOR('',#7066,0.225);
#1749=VECTOR('',#7073,0.225);
#1750=VECTOR('',#7080,0.225);
#1751=VECTOR('',#7087,0.225);
#1752=VECTOR('',#7094,2.34);
#1753=VECTOR('',#7105,1.8);
#1754=VECTOR('',#7110,3.5);
#1755=VECTOR('',#7121,1.);
#1756=VECTOR('',#7122,1.);
#1757=VECTOR('',#7123,1.);
#1758=VECTOR('',#7124,1.);
#1759=VECTOR('',#7127,1.);
#1760=VECTOR('',#7128,1.);
#1761=VECTOR('',#7129,1.);
#1762=VECTOR('',#7132,1.);
#1763=VECTOR('',#7133,1.);
#1764=VECTOR('',#7134,1.);
#1765=VECTOR('',#7137,1.);
#1766=VECTOR('',#7138,1.);
#1767=VECTOR('',#7147,1.);
#1768=VECTOR('',#7148,1.);
#1769=VECTOR('',#7149,1.);
#1770=VECTOR('',#7150,1.);
#1771=VECTOR('',#7153,1.);
#1772=VECTOR('',#7154,1.);
#1773=VECTOR('',#7155,1.);
#1774=VECTOR('',#7158,1.);
#1775=VECTOR('',#7159,1.);
#1776=VECTOR('',#7160,1.);
#1777=VECTOR('',#7163,1.);
#1778=VECTOR('',#7164,1.);
#1779=VECTOR('',#7187,1.63531);
#1780=VECTOR('',#7194,1.);
#1781=VECTOR('',#7199,1.05);
#1782=VECTOR('',#7208,1.63531);
#1783=VECTOR('',#7215,1.05);
#1784=VECTOR('',#7234,1.71469);
#1785=VECTOR('',#7245,2.3);
#1786=VECTOR('',#7250,2.35);
#1787=VECTOR('',#7255,2.3);
#1788=VECTOR('',#7260,1.71469);
#1789=VECTOR('',#7311,1.706752);
#1790=VECTOR('',#7388,1.643248);
#1791=VECTOR('',#7417,1.70469);
#1792=VECTOR('',#7424,1.65031);
#1793=VECTOR('',#7435,1.70469);
#1794=VECTOR('',#7442,1.65031);
#1795=VECTOR('',#7463,0.475);
#1796=VECTOR('',#7468,0.5);
#1797=VECTOR('',#7473,0.485);
#1798=VECTOR('',#7482,0.31);
#1799=VECTOR('',#7487,0.3);
#1800=VECTOR('',#7492,0.27);
#1801=VECTOR('',#7497,1.);
#1802=VECTOR('',#7498,1.);
#1803=VECTOR('',#7499,1.);
#1804=VECTOR('',#7500,1.);
#1805=VECTOR('',#7503,1.);
#1806=VECTOR('',#7504,1.);
#1807=VECTOR('',#7505,1.);
#1808=VECTOR('',#7508,1.);
#1809=VECTOR('',#7509,1.);
#1810=VECTOR('',#7510,1.);
#1811=VECTOR('',#7513,1.);
#1812=VECTOR('',#7514,1.);
#1813=VECTOR('',#7515,1.);
#1814=VECTOR('',#7518,1.);
#1815=VECTOR('',#7519,1.);
#1816=VECTOR('',#7520,1.);
#1817=VECTOR('',#7523,1.);
#1818=VECTOR('',#7524,1.);
#1819=VECTOR('',#7539,0.325);
#1820=VECTOR('',#7544,0.35);
#1821=VECTOR('',#7549,0.335);
#1822=VECTOR('',#7558,0.21);
#1823=VECTOR('',#7563,0.2);
#1824=VECTOR('',#7568,0.18);
#1825=VECTOR('',#7573,1.);
#1826=VECTOR('',#7574,1.);
#1827=VECTOR('',#7575,1.);
#1828=VECTOR('',#7576,1.);
#1829=VECTOR('',#7579,1.);
#1830=VECTOR('',#7580,1.);
#1831=VECTOR('',#7581,1.);
#1832=VECTOR('',#7584,1.);
#1833=VECTOR('',#7585,1.);
#1834=VECTOR('',#7586,1.);
#1835=VECTOR('',#7589,1.);
#1836=VECTOR('',#7590,1.);
#1837=VECTOR('',#7591,1.);
#1838=VECTOR('',#7594,1.);
#1839=VECTOR('',#7595,1.);
#1840=VECTOR('',#7596,1.);
#1841=VECTOR('',#7599,1.);
#1842=VECTOR('',#7600,1.);
#1843=VECTOR('',#7655,1.);
#1844=VECTOR('',#7656,1.);
#1845=VECTOR('',#7657,1.);
#1846=VECTOR('',#7658,1.);
#1847=VECTOR('',#7663,1.);
#1848=VECTOR('',#7664,1.);
#1849=VECTOR('',#7667,1.);
#1850=VECTOR('',#7668,1.);
#1851=VECTOR('',#7669,1.);
#1852=VECTOR('',#7672,1.);
#1853=VECTOR('',#7681,0.6);
#1854=VECTOR('',#7700,1.2);
#1855=VECTOR('',#7703,1.);
#1856=VECTOR('',#7710,1.);
#1857=VECTOR('',#7721,1.01);
#1858=VECTOR('',#7728,1.35);
#1859=VECTOR('',#7739,1.);
#1860=VECTOR('',#7746,0.21);
#1861=VECTOR('',#7751,1.);
#1862=VECTOR('',#7756,1.005);
#1863=VECTOR('',#7763,1.5);
#1864=VECTOR('',#7774,1.);
#1865=VECTOR('',#7781,0.21);
#1866=VECTOR('',#7786,1.);
#1867=VECTOR('',#7791,0.605);
#1868=VECTOR('',#7798,1.2);
#1869=VECTOR('',#7809,1.);
#1870=VECTOR('',#7810,1.);
#1871=VECTOR('',#7811,1.);
#1872=VECTOR('',#7812,1.);
#1873=VECTOR('',#7815,1.);
#1874=VECTOR('',#7816,1.);
#1875=VECTOR('',#7817,1.);
#1876=VECTOR('',#7822,1.);
#1877=VECTOR('',#7823,1.);
#1878=VECTOR('',#7824,1.);
#1879=VECTOR('',#7837,0.125);
#1880=VECTOR('',#7840,0.125);
#1881=VECTOR('',#7845,1.);
#1882=VECTOR('',#7846,1.);
#1883=VECTOR('',#7851,0.125);
#1884=VECTOR('',#7854,0.125);
#1885=VECTOR('',#8025,1.4);
#1886=VECTOR('',#8194,1.4);
#1887=VECTOR('',#8197,1.);
#1888=VECTOR('',#8198,1.);
#1889=VECTOR('',#8201,1.);
#1890=VECTOR('',#8204,1.);
#1891=VECTOR('',#8207,1.);
#1892=VECTOR('',#8210,1.);
#1893=VECTOR('',#8213,1.);
#1894=VECTOR('',#8216,1.);
#1895=VECTOR('',#8219,1.);
#1896=VECTOR('',#8222,1.);
#1897=VECTOR('',#8225,1.);
#1898=VECTOR('',#8228,1.);
#1899=VECTOR('',#8231,1.);
#1900=VECTOR('',#8234,1.);
#1901=VECTOR('',#8237,1.);
#1902=VECTOR('',#8240,1.);
#1903=VECTOR('',#8243,1.);
#1904=VECTOR('',#8246,1.);
#1905=VECTOR('',#8249,1.);
#1906=VECTOR('',#8252,1.);
#1907=VECTOR('',#8255,1.);
#1908=VECTOR('',#8258,1.);
#1909=VECTOR('',#8261,1.);
#1910=VECTOR('',#8264,1.);
#1911=VECTOR('',#8267,1.);
#1912=VECTOR('',#8270,1.);
#1913=VECTOR('',#8273,1.);
#1914=VECTOR('',#8276,1.);
#1915=VECTOR('',#8279,1.);
#1916=VECTOR('',#8282,1.);
#1917=VECTOR('',#8285,1.);
#1918=VECTOR('',#8288,1.);
#1919=VECTOR('',#8291,1.);
#1920=VECTOR('',#8294,1.);
#1921=VECTOR('',#8297,1.);
#1922=VECTOR('',#8300,1.);
#1923=VECTOR('',#8303,1.);
#1924=VECTOR('',#8306,1.);
#1925=VECTOR('',#8309,1.);
#1926=VECTOR('',#8312,1.);
#1927=VECTOR('',#8315,1.);
#1928=VECTOR('',#8318,1.);
#1929=VECTOR('',#8321,1.);
#1930=VECTOR('',#8324,1.);
#1931=VECTOR('',#8327,1.);
#1932=VECTOR('',#8330,1.);
#1933=VECTOR('',#8333,1.);
#1934=VECTOR('',#8336,1.);
#1935=VECTOR('',#8339,1.);
#1936=VECTOR('',#8342,1.);
#1937=VECTOR('',#8345,1.);
#1938=VECTOR('',#8348,1.);
#1939=VECTOR('',#8351,1.);
#1940=VECTOR('',#8354,1.);
#1941=VECTOR('',#8357,1.);
#1942=VECTOR('',#8360,1.);
#1943=VECTOR('',#8363,1.);
#1944=VECTOR('',#8366,1.);
#1945=VECTOR('',#8369,1.);
#1946=VECTOR('',#8372,1.);
#1947=VECTOR('',#8375,1.);
#1948=VECTOR('',#8378,1.);
#1949=VECTOR('',#8381,1.);
#1950=VECTOR('',#8384,1.);
#1951=VECTOR('',#8387,1.);
#1952=VECTOR('',#8390,1.);
#1953=VECTOR('',#8393,1.);
#1954=VECTOR('',#8396,1.);
#1955=VECTOR('',#8399,1.);
#1956=VECTOR('',#8402,1.);
#1957=VECTOR('',#8405,1.);
#1958=VECTOR('',#8408,1.);
#1959=VECTOR('',#8411,1.);
#1960=VECTOR('',#8414,1.);
#1961=VECTOR('',#8417,1.);
#1962=VECTOR('',#8420,1.);
#1963=VECTOR('',#8423,1.);
#1964=VECTOR('',#8426,1.);
#1965=VECTOR('',#8429,1.);
#1966=VECTOR('',#8432,1.);
#1967=VECTOR('',#8439,1.);
#1968=VECTOR('',#8440,1.);
#1969=VECTOR('',#8441,1.);
#1970=VECTOR('',#8442,1.);
#1971=VECTOR('',#8443,1.);
#1972=VECTOR('',#8444,1.);
#1973=VECTOR('',#8445,1.);
#1974=VECTOR('',#8446,1.);
#1975=VECTOR('',#8449,1.);
#1976=VECTOR('',#8450,1.);
#1977=VECTOR('',#8451,1.);
#1978=VECTOR('',#8454,1.);
#1979=VECTOR('',#8455,1.);
#1980=VECTOR('',#8458,1.);
#1981=VECTOR('',#8459,1.);
#1982=VECTOR('',#8462,1.);
#1983=VECTOR('',#8463,1.);
#1984=VECTOR('',#8466,1.);
#1985=VECTOR('',#8467,1.);
#1986=VECTOR('',#8468,1.);
#1987=VECTOR('',#8469,1.);
#1988=VECTOR('',#8472,1.);
#1989=VECTOR('',#8475,1.);
#1990=VECTOR('',#8478,1.);
#1991=VECTOR('',#8485,1.);
#1992=VECTOR('',#8486,1.);
#1993=VECTOR('',#8487,1.);
#1994=VECTOR('',#8488,1.);
#1995=VECTOR('',#8491,1.);
#1996=VECTOR('',#8492,1.);
#1997=VECTOR('',#8493,1.);
#1998=VECTOR('',#8496,1.);
#1999=VECTOR('',#8497,1.);
#2000=VECTOR('',#8498,1.);
#2001=VECTOR('',#8501,1.);
#2002=VECTOR('',#8502,1.);
#2003=VECTOR('',#8503,1.);
#2004=VECTOR('',#8506,1.);
#2005=VECTOR('',#8507,1.);
#2006=VECTOR('',#8508,1.);
#2007=VECTOR('',#8511,1.);
#2008=VECTOR('',#8512,1.);
#2009=VECTOR('',#8523,0.235);
#2010=VECTOR('',#8528,0.25);
#2011=VECTOR('',#8533,0.2125);
#2012=CIRCLE('',#5929,0.25);
#2013=CIRCLE('',#5930,0.25);
#2014=CIRCLE('',#5932,0.25);
#2015=CIRCLE('',#5933,0.25);
#2016=CIRCLE('',#5935,0.25);
#2017=CIRCLE('',#5936,0.25);
#2018=CIRCLE('',#5938,0.25);
#2019=CIRCLE('',#5939,0.25);
#2020=CIRCLE('',#5948,0.165);
#2021=CIRCLE('',#5949,0.165);
#2022=CIRCLE('',#5952,0.165);
#2023=CIRCLE('',#5953,0.165);
#2024=CIRCLE('',#5956,0.165);
#2025=CIRCLE('',#5957,0.165);
#2026=CIRCLE('',#5960,0.165);
#2027=CIRCLE('',#5961,0.165);
#2028=CIRCLE('',#5964,0.165);
#2029=CIRCLE('',#5965,0.165);
#2030=CIRCLE('',#5968,0.165);
#2031=CIRCLE('',#5969,0.165);
#2032=CIRCLE('',#5972,0.165);
#2033=CIRCLE('',#5973,0.165);
#2034=CIRCLE('',#5976,0.165);
#2035=CIRCLE('',#5977,0.165);
#2036=CIRCLE('',#5980,0.33);
#2037=CIRCLE('',#5981,0.33);
#2038=CIRCLE('',#5983,0.33);
#2039=CIRCLE('',#5984,0.33);
#2040=CIRCLE('',#5986,0.33);
#2041=CIRCLE('',#5987,0.33);
#2042=CIRCLE('',#5989,0.33);
#2043=CIRCLE('',#5990,0.33);
#2044=CIRCLE('',#5992,3.5);
#2045=CIRCLE('',#5994,3.5);
#2046=CIRCLE('',#5996,3.5);
#2047=CIRCLE('',#5998,3.5);
#2048=CIRCLE('',#6005,3.5);
#2049=CIRCLE('',#6007,3.5);
#2050=CIRCLE('',#6009,3.5);
#2051=CIRCLE('',#6011,3.5);
#2052=CIRCLE('',#6018,2.35);
#2053=CIRCLE('',#6019,2.35);
#2054=CIRCLE('',#6021,3.5);
#2055=CIRCLE('',#6022,3.5);
#2056=CIRCLE('',#6027,1.75);
#2057=CIRCLE('',#6028,1.75);
#2058=CIRCLE('',#6030,2.34);
#2059=CIRCLE('',#6031,2.34);
#2060=CIRCLE('',#6036,0.225);
#2061=CIRCLE('',#6037,0.225);
#2062=CIRCLE('',#6039,0.225);
#2063=CIRCLE('',#6040,0.225);
#2064=CIRCLE('',#6042,0.225);
#2065=CIRCLE('',#6043,0.225);
#2066=CIRCLE('',#6045,0.225);
#2067=CIRCLE('',#6046,0.225);
#2068=CIRCLE('',#6048,2.34);
#2069=CIRCLE('',#6049,2.34);
#2070=CIRCLE('',#6051,1.6);
#2071=CIRCLE('',#6053,1.8);
#2072=CIRCLE('',#6054,1.8);
#2073=CIRCLE('',#6056,1.6);
#2074=CIRCLE('',#6059,3.5);
#2075=CIRCLE('',#6060,3.5);
#2076=CIRCLE('',#6065,1.);
#2077=CIRCLE('',#6066,1.);
#2078=CIRCLE('',#6068,1.8);
#2079=CIRCLE('',#6069,1.8);
#2080=CIRCLE('',#6074,0.225);
#2081=CIRCLE('',#6075,0.225);
#2082=CIRCLE('',#6077,0.225);
#2083=CIRCLE('',#6078,0.225);
#2084=CIRCLE('',#6080,0.225);
#2085=CIRCLE('',#6081,0.225);
#2086=CIRCLE('',#6083,0.225);
#2087=CIRCLE('',#6084,0.225);
#2088=CIRCLE('',#6086,2.34);
#2089=CIRCLE('',#6087,2.34);
#2090=CIRCLE('',#6089,1.8);
#2091=CIRCLE('',#6091,1.8);
#2092=CIRCLE('',#6093,3.5);
#2093=CIRCLE('',#6094,3.5);
#2094=CIRCLE('',#6114,1.63531);
#2095=CIRCLE('',#6115,1.63531);
#2096=CIRCLE('',#6116,0.412776);
#2097=CIRCLE('',#6117,1.63531);
#2098=CIRCLE('',#6118,1.63531);
#2099=CIRCLE('',#6120,1.63531);
#2100=CIRCLE('',#6122,1.);
#2101=CIRCLE('',#6123,1.);
#2102=CIRCLE('',#6125,1.1);
#2103=CIRCLE('',#6128,1.63531);
#2104=CIRCLE('',#6130,1.1);
#2105=CIRCLE('',#6134,1.71469);
#2106=CIRCLE('',#6135,1.71469);
#2107=CIRCLE('',#6136,0.412776);
#2108=CIRCLE('',#6137,1.71469);
#2109=CIRCLE('',#6138,1.71469);
#2110=CIRCLE('',#6140,1.71469);
#2111=CIRCLE('',#6142,2.25);
#2112=CIRCLE('',#6143,1.71469);
#2113=CIRCLE('',#6145,2.35);
#2114=CIRCLE('',#6147,2.35);
#2115=CIRCLE('',#6149,2.25);
#2116=CIRCLE('',#6154,0.3969);
#2117=CIRCLE('',#6156,0.3969);
#2118=CIRCLE('',#6158,0.3969);
#2119=CIRCLE('',#6160,0.3969);
#2120=CIRCLE('',#6162,0.3969);
#2121=CIRCLE('',#6164,0.3969);
#2122=CIRCLE('',#6166,0.3969);
#2123=CIRCLE('',#6168,0.3969);
#2124=CIRCLE('',#6171,0.405071403305639);
#2125=CIRCLE('',#6172,0.405071403305639);
#2126=CIRCLE('',#6174,1.706752);
#2127=CIRCLE('',#6175,1.706752);
#2128=CIRCLE('',#6176,1.706752);
#2129=CIRCLE('',#6177,1.706752);
#2130=CIRCLE('',#6178,1.706752);
#2131=CIRCLE('',#6179,1.706752);
#2132=CIRCLE('',#6180,1.706752);
#2133=CIRCLE('',#6181,1.706752);
#2134=CIRCLE('',#6182,1.706752);
#2135=CIRCLE('',#6184,1.643248);
#2136=CIRCLE('',#6185,0.405071403305639);
#2137=CIRCLE('',#6187,0.405071403305639);
#2138=CIRCLE('',#6189,1.643248);
#2139=CIRCLE('',#6190,0.405071403305639);
#2140=CIRCLE('',#6192,0.405071403305639);
#2141=CIRCLE('',#6194,1.643248);
#2142=CIRCLE('',#6195,0.405071403305639);
#2143=CIRCLE('',#6197,0.405071403305639);
#2144=CIRCLE('',#6199,1.643248);
#2145=CIRCLE('',#6200,0.405071403305639);
#2146=CIRCLE('',#6202,0.405071403305639);
#2147=CIRCLE('',#6204,1.643248);
#2148=CIRCLE('',#6205,0.405071403305639);
#2149=CIRCLE('',#6207,0.405071403305639);
#2150=CIRCLE('',#6209,1.643248);
#2151=CIRCLE('',#6210,0.405071403305639);
#2152=CIRCLE('',#6212,0.405071403305639);
#2153=CIRCLE('',#6214,1.643248);
#2154=CIRCLE('',#6215,1.643248);
#2155=CIRCLE('',#6216,1.643248);
#2156=CIRCLE('',#6218,0.405071403305639);
#2157=CIRCLE('',#6220,0.405071403305639);
#2158=CIRCLE('',#6225,1.70469);
#2159=CIRCLE('',#6226,1.65031);
#2160=CIRCLE('',#6228,1.70469);
#2161=CIRCLE('',#6230,1.65031);
#2162=CIRCLE('',#6233,1.70469);
#2163=CIRCLE('',#6234,1.65031);
#2164=CIRCLE('',#6236,1.70469);
#2165=CIRCLE('',#6238,1.65031);
#2166=CIRCLE('',#6247,0.45);
#2167=CIRCLE('',#6249,0.5);
#2168=CIRCLE('',#6251,0.5);
#2169=CIRCLE('',#6253,0.47);
#2170=CIRCLE('',#6255,0.32);
#2171=CIRCLE('',#6257,0.2942);
#2172=CIRCLE('',#6259,0.2942);
#2173=CIRCLE('',#6261,0.24);
#2174=CIRCLE('',#6273,0.3);
#2175=CIRCLE('',#6275,0.35);
#2176=CIRCLE('',#6277,0.35);
#2177=CIRCLE('',#6279,0.32);
#2178=CIRCLE('',#6281,0.22);
#2179=CIRCLE('',#6283,0.1954);
#2180=CIRCLE('',#6285,0.1954);
#2181=CIRCLE('',#6287,0.16);
#2182=CIRCLE('',#6323,0.6);
#2183=CIRCLE('',#6327,0.6);
#2184=CIRCLE('',#6329,0.6);
#2185=CIRCLE('',#6330,0.6);
#2186=CIRCLE('',#6333,1.2);
#2187=CIRCLE('',#6334,1.);
#2188=CIRCLE('',#6336,1.2);
#2189=CIRCLE('',#6337,1.);
#2190=CIRCLE('',#6340,1.);
#2191=CIRCLE('',#6342,1.);
#2192=CIRCLE('',#6347,1.01);
#2193=CIRCLE('',#6348,1.01);
#2194=CIRCLE('',#6350,1.35);
#2195=CIRCLE('',#6351,1.35);
#2196=CIRCLE('',#6356,0.21);
#2197=CIRCLE('',#6358,0.21);
#2198=CIRCLE('',#6359,0.21);
#2199=CIRCLE('',#6362,1.005);
#2200=CIRCLE('',#6363,1.005);
#2201=CIRCLE('',#6365,1.5);
#2202=CIRCLE('',#6366,1.5);
#2203=CIRCLE('',#6371,0.21);
#2204=CIRCLE('',#6373,0.21);
#2205=CIRCLE('',#6374,0.21);
#2206=CIRCLE('',#6377,0.605);
#2207=CIRCLE('',#6378,0.605);
#2208=CIRCLE('',#6380,1.2);
#2209=CIRCLE('',#6381,1.2);
#2210=CIRCLE('',#6387,0.125);
#2211=CIRCLE('',#6390,1.4);
#2212=CIRCLE('',#6391,0.6);
#2213=CIRCLE('',#6393,0.6);
#2214=CIRCLE('',#6397,1.);
#2215=CIRCLE('',#6398,1.);
#2216=CIRCLE('',#6403,1.4);
#2217=CIRCLE('',#6404,0.0555000000000001);
#2218=CIRCLE('',#6405,1.24783954473516);
#2219=CIRCLE('',#6406,0.0555000000000001);
#2220=CIRCLE('',#6407,1.24783954473516);
#2221=CIRCLE('',#6408,0.0555000000000001);
#2222=CIRCLE('',#6409,1.24783954473516);
#2223=CIRCLE('',#6410,0.0555000000000001);
#2224=CIRCLE('',#6411,1.24783954473516);
#2225=CIRCLE('',#6412,0.0555000000000001);
#2226=CIRCLE('',#6413,1.24783954473516);
#2227=CIRCLE('',#6414,0.0555000000000001);
#2228=CIRCLE('',#6415,1.24783954473516);
#2229=CIRCLE('',#6416,0.0555000000000001);
#2230=CIRCLE('',#6417,1.24783954473516);
#2231=CIRCLE('',#6418,0.0555000000000001);
#2232=CIRCLE('',#6419,1.24783954473516);
#2233=CIRCLE('',#6420,0.0555000000000001);
#2234=CIRCLE('',#6421,1.24783954473516);
#2235=CIRCLE('',#6422,0.0555000000000001);
#2236=CIRCLE('',#6423,1.24783954473516);
#2237=CIRCLE('',#6424,0.0555000000000001);
#2238=CIRCLE('',#6425,1.24783954473516);
#2239=CIRCLE('',#6426,0.0555000000000001);
#2240=CIRCLE('',#6427,1.24783954473516);
#2241=CIRCLE('',#6428,0.0555000000000001);
#2242=CIRCLE('',#6429,1.24783954473516);
#2243=CIRCLE('',#6430,0.0555000000000001);
#2244=CIRCLE('',#6431,1.24783954473516);
#2245=CIRCLE('',#6432,0.0555000000000001);
#2246=CIRCLE('',#6433,1.24783954473516);
#2247=CIRCLE('',#6434,0.0555000000000001);
#2248=CIRCLE('',#6435,1.24783954473516);
#2249=CIRCLE('',#6436,0.0555000000000001);
#2250=CIRCLE('',#6437,1.24783954473516);
#2251=CIRCLE('',#6438,0.0555000000000001);
#2252=CIRCLE('',#6439,1.24783954473516);
#2253=CIRCLE('',#6440,0.0555000000000001);
#2254=CIRCLE('',#6441,1.24783954473516);
#2255=CIRCLE('',#6442,0.0555000000000001);
#2256=CIRCLE('',#6443,1.24783954473516);
#2257=CIRCLE('',#6444,0.0555000000000001);
#2258=CIRCLE('',#6445,1.24783954473516);
#2259=CIRCLE('',#6446,0.0555000000000001);
#2260=CIRCLE('',#6447,1.24783954473516);
#2261=CIRCLE('',#6448,0.0555000000000001);
#2262=CIRCLE('',#6449,1.24783954473516);
#2263=CIRCLE('',#6450,0.0555000000000001);
#2264=CIRCLE('',#6451,1.24783954473516);
#2265=CIRCLE('',#6452,0.0555000000000001);
#2266=CIRCLE('',#6453,1.24783954473516);
#2267=CIRCLE('',#6454,0.0555000000000001);
#2268=CIRCLE('',#6455,1.24783954473516);
#2269=CIRCLE('',#6456,0.0555000000000001);
#2270=CIRCLE('',#6457,1.24783954473516);
#2271=CIRCLE('',#6458,0.0555000000000001);
#2272=CIRCLE('',#6459,1.24783954473516);
#2273=CIRCLE('',#6460,0.0555000000000001);
#2274=CIRCLE('',#6461,1.24783954473516);
#2275=CIRCLE('',#6462,0.0555000000000001);
#2276=CIRCLE('',#6463,1.24783954473516);
#2277=CIRCLE('',#6464,0.0555000000000001);
#2278=CIRCLE('',#6465,1.24783954473516);
#2279=CIRCLE('',#6466,0.0555000000000001);
#2280=CIRCLE('',#6467,1.24783954473516);
#2281=CIRCLE('',#6468,0.0555000000000001);
#2282=CIRCLE('',#6469,1.24783954473516);
#2283=CIRCLE('',#6470,0.0555000000000001);
#2284=CIRCLE('',#6471,1.24783954473516);
#2285=CIRCLE('',#6472,0.0555000000000001);
#2286=CIRCLE('',#6473,1.24783954473516);
#2287=CIRCLE('',#6474,0.0555000000000001);
#2288=CIRCLE('',#6475,1.24783954473516);
#2289=CIRCLE('',#6476,0.0555000000000001);
#2290=CIRCLE('',#6477,1.24783954473516);
#2291=CIRCLE('',#6478,0.0555000000000001);
#2292=CIRCLE('',#6479,1.24783954473516);
#2293=CIRCLE('',#6480,0.0555000000000001);
#2294=CIRCLE('',#6481,1.24783954473516);
#2295=CIRCLE('',#6482,0.0555000000000001);
#2296=CIRCLE('',#6483,1.24783954473516);
#2297=CIRCLE('',#6485,1.4);
#2298=CIRCLE('',#6488,1.4);
#2299=CIRCLE('',#6489,0.0555000000000001);
#2300=CIRCLE('',#6490,1.24783954473516);
#2301=CIRCLE('',#6491,0.0555000000000001);
#2302=CIRCLE('',#6492,1.24783954473516);
#2303=CIRCLE('',#6493,0.0555000000000001);
#2304=CIRCLE('',#6494,1.24783954473516);
#2305=CIRCLE('',#6495,0.0555000000000001);
#2306=CIRCLE('',#6496,1.24783954473516);
#2307=CIRCLE('',#6497,0.0555000000000001);
#2308=CIRCLE('',#6498,1.24783954473516);
#2309=CIRCLE('',#6499,0.0555000000000001);
#2310=CIRCLE('',#6500,1.24783954473516);
#2311=CIRCLE('',#6501,0.0555000000000001);
#2312=CIRCLE('',#6502,1.24783954473516);
#2313=CIRCLE('',#6503,0.0555000000000001);
#2314=CIRCLE('',#6504,1.24783954473516);
#2315=CIRCLE('',#6505,0.0555000000000001);
#2316=CIRCLE('',#6506,1.24783954473516);
#2317=CIRCLE('',#6507,0.0555000000000001);
#2318=CIRCLE('',#6508,1.24783954473516);
#2319=CIRCLE('',#6509,0.0555000000000001);
#2320=CIRCLE('',#6510,1.24783954473516);
#2321=CIRCLE('',#6511,0.0555000000000001);
#2322=CIRCLE('',#6512,1.24783954473516);
#2323=CIRCLE('',#6513,0.0555000000000001);
#2324=CIRCLE('',#6514,1.24783954473516);
#2325=CIRCLE('',#6515,0.0555000000000001);
#2326=CIRCLE('',#6516,1.24783954473516);
#2327=CIRCLE('',#6517,0.0555000000000001);
#2328=CIRCLE('',#6518,1.24783954473516);
#2329=CIRCLE('',#6519,0.0555000000000001);
#2330=CIRCLE('',#6520,1.24783954473516);
#2331=CIRCLE('',#6521,0.0555000000000001);
#2332=CIRCLE('',#6522,1.24783954473516);
#2333=CIRCLE('',#6523,0.0555000000000001);
#2334=CIRCLE('',#6524,1.24783954473516);
#2335=CIRCLE('',#6525,0.0555000000000001);
#2336=CIRCLE('',#6526,1.24783954473516);
#2337=CIRCLE('',#6527,0.0555000000000001);
#2338=CIRCLE('',#6528,1.24783954473516);
#2339=CIRCLE('',#6529,0.0555000000000001);
#2340=CIRCLE('',#6530,1.24783954473516);
#2341=CIRCLE('',#6531,0.0555000000000001);
#2342=CIRCLE('',#6532,1.24783954473516);
#2343=CIRCLE('',#6533,0.0555000000000001);
#2344=CIRCLE('',#6534,1.24783954473516);
#2345=CIRCLE('',#6535,0.0555000000000001);
#2346=CIRCLE('',#6536,1.24783954473516);
#2347=CIRCLE('',#6537,0.0555000000000001);
#2348=CIRCLE('',#6538,1.24783954473516);
#2349=CIRCLE('',#6539,0.0555000000000001);
#2350=CIRCLE('',#6540,1.24783954473516);
#2351=CIRCLE('',#6541,0.0555000000000001);
#2352=CIRCLE('',#6542,1.24783954473516);
#2353=CIRCLE('',#6543,0.0555000000000001);
#2354=CIRCLE('',#6544,1.24783954473516);
#2355=CIRCLE('',#6545,0.0555000000000001);
#2356=CIRCLE('',#6546,1.24783954473516);
#2357=CIRCLE('',#6547,0.0555000000000001);
#2358=CIRCLE('',#6548,1.24783954473516);
#2359=CIRCLE('',#6549,0.0555000000000001);
#2360=CIRCLE('',#6550,1.24783954473516);
#2361=CIRCLE('',#6551,0.0555000000000001);
#2362=CIRCLE('',#6552,1.24783954473516);
#2363=CIRCLE('',#6553,0.0555000000000001);
#2364=CIRCLE('',#6554,1.24783954473516);
#2365=CIRCLE('',#6555,0.0555000000000001);
#2366=CIRCLE('',#6556,1.24783954473516);
#2367=CIRCLE('',#6557,0.0555000000000001);
#2368=CIRCLE('',#6558,1.24783954473516);
#2369=CIRCLE('',#6559,0.0555000000000001);
#2370=CIRCLE('',#6560,1.24783954473516);
#2371=CIRCLE('',#6561,0.0555000000000001);
#2372=CIRCLE('',#6562,1.24783954473516);
#2373=CIRCLE('',#6563,0.0555000000000001);
#2374=CIRCLE('',#6564,1.24783954473516);
#2375=CIRCLE('',#6565,0.0555000000000001);
#2376=CIRCLE('',#6566,1.24783954473516);
#2377=CIRCLE('',#6567,0.0555000000000001);
#2378=CIRCLE('',#6568,1.24783954473516);
#2379=CIRCLE('',#6670,0.22);
#2380=CIRCLE('',#6672,0.24505);
#2381=CIRCLE('',#6674,0.24505);
#2382=CIRCLE('',#6676,0.175);
#2383=VERTEX_POINT('',#8560);
#2384=VERTEX_POINT('',#8562);
#2385=VERTEX_POINT('',#8566);
#2386=VERTEX_POINT('',#8568);
#2387=VERTEX_POINT('',#8572);
#2388=VERTEX_POINT('',#8574);
#2389=VERTEX_POINT('',#8578);
#2390=VERTEX_POINT('',#8580);
#2391=VERTEX_POINT('',#8584);
#2392=VERTEX_POINT('',#8585);
#2393=VERTEX_POINT('',#8587);
#2394=VERTEX_POINT('',#8589);
#2395=VERTEX_POINT('',#8593);
#2396=VERTEX_POINT('',#8595);
#2397=VERTEX_POINT('',#8599);
#2398=VERTEX_POINT('',#8601);
#2399=VERTEX_POINT('',#8611);
#2400=VERTEX_POINT('',#8613);
#2401=VERTEX_POINT('',#8618);
#2402=VERTEX_POINT('',#8620);
#2403=VERTEX_POINT('',#8625);
#2404=VERTEX_POINT('',#8627);
#2405=VERTEX_POINT('',#8632);
#2406=VERTEX_POINT('',#8634);
#2407=VERTEX_POINT('',#8639);
#2408=VERTEX_POINT('',#8641);
#2409=VERTEX_POINT('',#8646);
#2410=VERTEX_POINT('',#8648);
#2411=VERTEX_POINT('',#8653);
#2412=VERTEX_POINT('',#8655);
#2413=VERTEX_POINT('',#8660);
#2414=VERTEX_POINT('',#8662);
#2415=VERTEX_POINT('',#8667);
#2416=VERTEX_POINT('',#8669);
#2417=VERTEX_POINT('',#8673);
#2418=VERTEX_POINT('',#8675);
#2419=VERTEX_POINT('',#8679);
#2420=VERTEX_POINT('',#8681);
#2421=VERTEX_POINT('',#8685);
#2422=VERTEX_POINT('',#8687);
#2423=VERTEX_POINT('',#8691);
#2424=VERTEX_POINT('',#8692);
#2425=VERTEX_POINT('',#8694);
#2426=VERTEX_POINT('',#8696);
#2427=VERTEX_POINT('',#8700);
#2428=VERTEX_POINT('',#8702);
#2429=VERTEX_POINT('',#8704);
#2430=VERTEX_POINT('',#8708);
#2431=VERTEX_POINT('',#8709);
#2432=VERTEX_POINT('',#8711);
#2433=VERTEX_POINT('',#8713);
#2434=VERTEX_POINT('',#8717);
#2435=VERTEX_POINT('',#8719);
#2436=VERTEX_POINT('',#8721);
#2437=VERTEX_POINT('',#8736);
#2438=VERTEX_POINT('',#8737);
#2439=VERTEX_POINT('',#8739);
#2440=VERTEX_POINT('',#8741);
#2441=VERTEX_POINT('',#8745);
#2442=VERTEX_POINT('',#8747);
#2443=VERTEX_POINT('',#8749);
#2444=VERTEX_POINT('',#8753);
#2445=VERTEX_POINT('',#8754);
#2446=VERTEX_POINT('',#8756);
#2447=VERTEX_POINT('',#8758);
#2448=VERTEX_POINT('',#8762);
#2449=VERTEX_POINT('',#8764);
#2450=VERTEX_POINT('',#8766);
#2451=VERTEX_POINT('',#8781);
#2452=VERTEX_POINT('',#8783);
#2453=VERTEX_POINT('',#8787);
#2454=VERTEX_POINT('',#8789);
#2455=VERTEX_POINT('',#8796);
#2456=VERTEX_POINT('',#8798);
#2457=VERTEX_POINT('',#8802);
#2458=VERTEX_POINT('',#8804);
#2459=VERTEX_POINT('',#8811);
#2460=VERTEX_POINT('',#8813);
#2461=VERTEX_POINT('',#8817);
#2462=VERTEX_POINT('',#8819);
#2463=VERTEX_POINT('',#8823);
#2464=VERTEX_POINT('',#8825);
#2465=VERTEX_POINT('',#8829);
#2466=VERTEX_POINT('',#8831);
#2467=VERTEX_POINT('',#8835);
#2468=VERTEX_POINT('',#8837);
#2469=VERTEX_POINT('',#8841);
#2470=VERTEX_POINT('',#8844);
#2471=VERTEX_POINT('',#8846);
#2472=VERTEX_POINT('',#8850);
#2473=VERTEX_POINT('',#8855);
#2474=VERTEX_POINT('',#8857);
#2475=VERTEX_POINT('',#8864);
#2476=VERTEX_POINT('',#8866);
#2477=VERTEX_POINT('',#8870);
#2478=VERTEX_POINT('',#8872);
#2479=VERTEX_POINT('',#8879);
#2480=VERTEX_POINT('',#8881);
#2481=VERTEX_POINT('',#8885);
#2482=VERTEX_POINT('',#8887);
#2483=VERTEX_POINT('',#8891);
#2484=VERTEX_POINT('',#8893);
#2485=VERTEX_POINT('',#8897);
#2486=VERTEX_POINT('',#8899);
#2487=VERTEX_POINT('',#8903);
#2488=VERTEX_POINT('',#8905);
#2489=VERTEX_POINT('',#8909);
#2490=VERTEX_POINT('',#8912);
#2491=VERTEX_POINT('',#8916);
#2492=VERTEX_POINT('',#8918);
#2493=VERTEX_POINT('',#8925);
#2494=VERTEX_POINT('',#8926);
#2495=VERTEX_POINT('',#8928);
#2496=VERTEX_POINT('',#8930);
#2497=VERTEX_POINT('',#8934);
#2498=VERTEX_POINT('',#8936);
#2499=VERTEX_POINT('',#8940);
#2500=VERTEX_POINT('',#8942);
#2501=VERTEX_POINT('',#8952);
#2502=VERTEX_POINT('',#8953);
#2503=VERTEX_POINT('',#8955);
#2504=VERTEX_POINT('',#8957);
#2505=VERTEX_POINT('',#8961);
#2506=VERTEX_POINT('',#8963);
#2507=VERTEX_POINT('',#8967);
#2508=VERTEX_POINT('',#8969);
#2509=VERTEX_POINT('',#8980);
#2510=VERTEX_POINT('',#8981);
#2511=VERTEX_POINT('',#8984);
#2512=VERTEX_POINT('',#8986);
#2513=VERTEX_POINT('',#8990);
#2514=VERTEX_POINT('',#8994);
#2515=VERTEX_POINT('',#8996);
#2516=VERTEX_POINT('',#9000);
#2517=VERTEX_POINT('',#9005);
#2518=VERTEX_POINT('',#9009);
#2519=VERTEX_POINT('',#9015);
#2520=VERTEX_POINT('',#9016);
#2521=VERTEX_POINT('',#9019);
#2522=VERTEX_POINT('',#9021);
#2523=VERTEX_POINT('',#9025);
#2524=VERTEX_POINT('',#9029);
#2525=VERTEX_POINT('',#9031);
#2526=VERTEX_POINT('',#9034);
#2527=VERTEX_POINT('',#9038);
#2528=VERTEX_POINT('',#9042);
#2529=VERTEX_POINT('',#9050);
#2530=VERTEX_POINT('',#9051);
#2531=VERTEX_POINT('',#9054);
#2532=VERTEX_POINT('',#9055);
#2533=VERTEX_POINT('',#9058);
#2534=VERTEX_POINT('',#9059);
#2535=VERTEX_POINT('',#9062);
#2536=VERTEX_POINT('',#9063);
#2537=VERTEX_POINT('',#9066);
#2538=VERTEX_POINT('',#9067);
#2539=VERTEX_POINT('',#9070);
#2540=VERTEX_POINT('',#9071);
#2541=VERTEX_POINT('',#9074);
#2542=VERTEX_POINT('',#9075);
#2543=VERTEX_POINT('',#9078);
#2544=VERTEX_POINT('',#9079);
#2545=VERTEX_POINT('',#9083);
#2546=VERTEX_POINT('',#9084);
#2547=VERTEX_POINT('',#9107);
#2548=VERTEX_POINT('',#9109);
#2549=VERTEX_POINT('',#9134);
#2550=VERTEX_POINT('',#9136);
#2551=VERTEX_POINT('',#9159);
#2552=VERTEX_POINT('',#9161);
#2553=VERTEX_POINT('',#9184);
#2554=VERTEX_POINT('',#9186);
#2555=VERTEX_POINT('',#9199);
#2556=VERTEX_POINT('',#9202);
#2557=VERTEX_POINT('',#9215);
#2558=VERTEX_POINT('',#9217);
#2559=VERTEX_POINT('',#9240);
#2560=VERTEX_POINT('',#9242);
#2561=VERTEX_POINT('',#9265);
#2562=VERTEX_POINT('',#9267);
#2563=VERTEX_POINT('',#9290);
#2564=VERTEX_POINT('',#9292);
#2565=VERTEX_POINT('',#9317);
#2566=VERTEX_POINT('',#9321);
#2567=VERTEX_POINT('',#9346);
#2568=VERTEX_POINT('',#9350);
#2569=VERTEX_POINT('',#9375);
#2570=VERTEX_POINT('',#9379);
#2571=VERTEX_POINT('',#9380);
#2572=VERTEX_POINT('',#9407);
#2573=VERTEX_POINT('',#9411);
#2574=VERTEX_POINT('',#9436);
#2575=VERTEX_POINT('',#9440);
#2576=VERTEX_POINT('',#9465);
#2577=VERTEX_POINT('',#9469);
#2578=VERTEX_POINT('',#9494);
#2579=VERTEX_POINT('',#9497);
#2580=VERTEX_POINT('',#9499);
#2581=VERTEX_POINT('',#9531);
#2582=VERTEX_POINT('',#9533);
#2583=VERTEX_POINT('',#9536);
#2584=VERTEX_POINT('',#9540);
#2585=VERTEX_POINT('',#9545);
#2586=VERTEX_POINT('',#9547);
#2587=VERTEX_POINT('',#9550);
#2588=VERTEX_POINT('',#9554);
#2589=VERTEX_POINT('',#9565);
#2590=VERTEX_POINT('',#9568);
#2591=VERTEX_POINT('',#9572);
#2592=VERTEX_POINT('',#9576);
#2593=VERTEX_POINT('',#9580);
#2594=VERTEX_POINT('',#9583);
#2595=VERTEX_POINT('',#9587);
#2596=VERTEX_POINT('',#9591);
#2597=VERTEX_POINT('',#9596);
#2598=VERTEX_POINT('',#9597);
#2599=VERTEX_POINT('',#9599);
#2600=VERTEX_POINT('',#9601);
#2601=VERTEX_POINT('',#9605);
#2602=VERTEX_POINT('',#9607);
#2603=VERTEX_POINT('',#9611);
#2604=VERTEX_POINT('',#9613);
#2605=VERTEX_POINT('',#9617);
#2606=VERTEX_POINT('',#9619);
#2607=VERTEX_POINT('',#9623);
#2608=VERTEX_POINT('',#9625);
#2609=VERTEX_POINT('',#9635);
#2610=VERTEX_POINT('',#9638);
#2611=VERTEX_POINT('',#9642);
#2612=VERTEX_POINT('',#9646);
#2613=VERTEX_POINT('',#9650);
#2614=VERTEX_POINT('',#9653);
#2615=VERTEX_POINT('',#9657);
#2616=VERTEX_POINT('',#9661);
#2617=VERTEX_POINT('',#9666);
#2618=VERTEX_POINT('',#9667);
#2619=VERTEX_POINT('',#9669);
#2620=VERTEX_POINT('',#9671);
#2621=VERTEX_POINT('',#9675);
#2622=VERTEX_POINT('',#9677);
#2623=VERTEX_POINT('',#9681);
#2624=VERTEX_POINT('',#9683);
#2625=VERTEX_POINT('',#9687);
#2626=VERTEX_POINT('',#9689);
#2627=VERTEX_POINT('',#9693);
#2628=VERTEX_POINT('',#9695);
#2629=VERTEX_POINT('',#9728);
#2630=VERTEX_POINT('',#9729);
#2631=VERTEX_POINT('',#9731);
#2632=VERTEX_POINT('',#9733);
#2633=VERTEX_POINT('',#9737);
#2634=VERTEX_POINT('',#9739);
#2635=VERTEX_POINT('',#9743);
#2636=VERTEX_POINT('',#9745);
#2637=VERTEX_POINT('',#9753);
#2638=VERTEX_POINT('',#9755);
#2639=VERTEX_POINT('',#9760);
#2640=VERTEX_POINT('',#9762);
#2641=VERTEX_POINT('',#9765);
#2642=VERTEX_POINT('',#9767);
#2643=VERTEX_POINT('',#9772);
#2644=VERTEX_POINT('',#9776);
#2645=VERTEX_POINT('',#9783);
#2646=VERTEX_POINT('',#9785);
#2647=VERTEX_POINT('',#9789);
#2648=VERTEX_POINT('',#9791);
#2649=VERTEX_POINT('',#9798);
#2650=VERTEX_POINT('',#9799);
#2651=VERTEX_POINT('',#9803);
#2652=VERTEX_POINT('',#9818);
#2653=VERTEX_POINT('',#9820);
#2654=VERTEX_POINT('',#9822);
#2655=VERTEX_POINT('',#9859);
#2656=VERTEX_POINT('',#9878);
#2657=VERTEX_POINT('',#9880);
#2658=VERTEX_POINT('',#9884);
#2659=VERTEX_POINT('',#9886);
#2660=VERTEX_POINT('',#9893);
#2661=VERTEX_POINT('',#9894);
#2662=VERTEX_POINT('',#9898);
#2663=VERTEX_POINT('',#9909);
#2664=VERTEX_POINT('',#9911);
#2665=VERTEX_POINT('',#9913);
#2666=VERTEX_POINT('',#9950);
#2667=VERTEX_POINT('',#9965);
#2668=VERTEX_POINT('',#9967);
#2669=VERTEX_POINT('',#9971);
#2670=VERTEX_POINT('',#9973);
#2671=VERTEX_POINT('',#9980);
#2672=VERTEX_POINT('',#9981);
#2673=VERTEX_POINT('',#9983);
#2674=VERTEX_POINT('',#9985);
#2675=VERTEX_POINT('',#9989);
#2676=VERTEX_POINT('',#9991);
#2677=VERTEX_POINT('',#9994);
#2678=VERTEX_POINT('',#9997);
#2679=VERTEX_POINT('',#9999);
#2680=VERTEX_POINT('',#10003);
#2681=VERTEX_POINT('',#10008);
#2682=VERTEX_POINT('',#10009);
#2683=VERTEX_POINT('',#10046);
#2684=VERTEX_POINT('',#10047);
#2685=VERTEX_POINT('',#10084);
#2686=VERTEX_POINT('',#10085);
#2687=VERTEX_POINT('',#10123);
#2688=VERTEX_POINT('',#10124);
#2689=VERTEX_POINT('',#10135);
#2690=VERTEX_POINT('',#10166);
#2691=VERTEX_POINT('',#10168);
#2692=VERTEX_POINT('',#10179);
#2693=VERTEX_POINT('',#10209);
#2694=VERTEX_POINT('',#10212);
#2695=VERTEX_POINT('',#10215);
#2696=VERTEX_POINT('',#10216);
#2697=VERTEX_POINT('',#10235);
#2698=VERTEX_POINT('',#10256);
#2699=VERTEX_POINT('',#10257);
#2700=VERTEX_POINT('',#10276);
#2701=VERTEX_POINT('',#10303);
#2702=VERTEX_POINT('',#10305);
#2703=VERTEX_POINT('',#10306);
#2704=VERTEX_POINT('',#10308);
#2705=VERTEX_POINT('',#10310);
#2706=VERTEX_POINT('',#10312);
#2707=VERTEX_POINT('',#10314);
#2708=VERTEX_POINT('',#10316);
#2709=VERTEX_POINT('',#10318);
#2710=VERTEX_POINT('',#10320);
#2711=VERTEX_POINT('',#10322);
#2712=VERTEX_POINT('',#10324);
#2713=VERTEX_POINT('',#10326);
#2714=VERTEX_POINT('',#10328);
#2715=VERTEX_POINT('',#10330);
#2716=VERTEX_POINT('',#10332);
#2717=VERTEX_POINT('',#10334);
#2718=VERTEX_POINT('',#10336);
#2719=VERTEX_POINT('',#10338);
#2720=VERTEX_POINT('',#10340);
#2721=VERTEX_POINT('',#10342);
#2722=VERTEX_POINT('',#10344);
#2723=VERTEX_POINT('',#10346);
#2724=VERTEX_POINT('',#10348);
#2725=VERTEX_POINT('',#10350);
#2726=VERTEX_POINT('',#10352);
#2727=VERTEX_POINT('',#10354);
#2728=VERTEX_POINT('',#10356);
#2729=VERTEX_POINT('',#10358);
#2730=VERTEX_POINT('',#10360);
#2731=VERTEX_POINT('',#10362);
#2732=VERTEX_POINT('',#10364);
#2733=VERTEX_POINT('',#10366);
#2734=VERTEX_POINT('',#10368);
#2735=VERTEX_POINT('',#10370);
#2736=VERTEX_POINT('',#10372);
#2737=VERTEX_POINT('',#10374);
#2738=VERTEX_POINT('',#10376);
#2739=VERTEX_POINT('',#10378);
#2740=VERTEX_POINT('',#10380);
#2741=VERTEX_POINT('',#10382);
#2742=VERTEX_POINT('',#10384);
#2743=VERTEX_POINT('',#10386);
#2744=VERTEX_POINT('',#10388);
#2745=VERTEX_POINT('',#10390);
#2746=VERTEX_POINT('',#10392);
#2747=VERTEX_POINT('',#10394);
#2748=VERTEX_POINT('',#10396);
#2749=VERTEX_POINT('',#10398);
#2750=VERTEX_POINT('',#10400);
#2751=VERTEX_POINT('',#10402);
#2752=VERTEX_POINT('',#10404);
#2753=VERTEX_POINT('',#10406);
#2754=VERTEX_POINT('',#10408);
#2755=VERTEX_POINT('',#10410);
#2756=VERTEX_POINT('',#10412);
#2757=VERTEX_POINT('',#10414);
#2758=VERTEX_POINT('',#10416);
#2759=VERTEX_POINT('',#10418);
#2760=VERTEX_POINT('',#10420);
#2761=VERTEX_POINT('',#10422);
#2762=VERTEX_POINT('',#10424);
#2763=VERTEX_POINT('',#10426);
#2764=VERTEX_POINT('',#10428);
#2765=VERTEX_POINT('',#10430);
#2766=VERTEX_POINT('',#10432);
#2767=VERTEX_POINT('',#10434);
#2768=VERTEX_POINT('',#10436);
#2769=VERTEX_POINT('',#10438);
#2770=VERTEX_POINT('',#10440);
#2771=VERTEX_POINT('',#10442);
#2772=VERTEX_POINT('',#10444);
#2773=VERTEX_POINT('',#10446);
#2774=VERTEX_POINT('',#10448);
#2775=VERTEX_POINT('',#10450);
#2776=VERTEX_POINT('',#10452);
#2777=VERTEX_POINT('',#10454);
#2778=VERTEX_POINT('',#10456);
#2779=VERTEX_POINT('',#10458);
#2780=VERTEX_POINT('',#10460);
#2781=VERTEX_POINT('',#10462);
#2782=VERTEX_POINT('',#10466);
#2783=VERTEX_POINT('',#10471);
#2784=VERTEX_POINT('',#10473);
#2785=VERTEX_POINT('',#10474);
#2786=VERTEX_POINT('',#10476);
#2787=VERTEX_POINT('',#10478);
#2788=VERTEX_POINT('',#10480);
#2789=VERTEX_POINT('',#10482);
#2790=VERTEX_POINT('',#10484);
#2791=VERTEX_POINT('',#10486);
#2792=VERTEX_POINT('',#10488);
#2793=VERTEX_POINT('',#10490);
#2794=VERTEX_POINT('',#10492);
#2795=VERTEX_POINT('',#10494);
#2796=VERTEX_POINT('',#10496);
#2797=VERTEX_POINT('',#10498);
#2798=VERTEX_POINT('',#10500);
#2799=VERTEX_POINT('',#10502);
#2800=VERTEX_POINT('',#10504);
#2801=VERTEX_POINT('',#10506);
#2802=VERTEX_POINT('',#10508);
#2803=VERTEX_POINT('',#10510);
#2804=VERTEX_POINT('',#10512);
#2805=VERTEX_POINT('',#10514);
#2806=VERTEX_POINT('',#10516);
#2807=VERTEX_POINT('',#10518);
#2808=VERTEX_POINT('',#10520);
#2809=VERTEX_POINT('',#10522);
#2810=VERTEX_POINT('',#10524);
#2811=VERTEX_POINT('',#10526);
#2812=VERTEX_POINT('',#10528);
#2813=VERTEX_POINT('',#10530);
#2814=VERTEX_POINT('',#10532);
#2815=VERTEX_POINT('',#10534);
#2816=VERTEX_POINT('',#10536);
#2817=VERTEX_POINT('',#10538);
#2818=VERTEX_POINT('',#10540);
#2819=VERTEX_POINT('',#10542);
#2820=VERTEX_POINT('',#10544);
#2821=VERTEX_POINT('',#10546);
#2822=VERTEX_POINT('',#10548);
#2823=VERTEX_POINT('',#10550);
#2824=VERTEX_POINT('',#10552);
#2825=VERTEX_POINT('',#10554);
#2826=VERTEX_POINT('',#10556);
#2827=VERTEX_POINT('',#10558);
#2828=VERTEX_POINT('',#10560);
#2829=VERTEX_POINT('',#10562);
#2830=VERTEX_POINT('',#10564);
#2831=VERTEX_POINT('',#10566);
#2832=VERTEX_POINT('',#10568);
#2833=VERTEX_POINT('',#10570);
#2834=VERTEX_POINT('',#10572);
#2835=VERTEX_POINT('',#10574);
#2836=VERTEX_POINT('',#10576);
#2837=VERTEX_POINT('',#10578);
#2838=VERTEX_POINT('',#10580);
#2839=VERTEX_POINT('',#10582);
#2840=VERTEX_POINT('',#10584);
#2841=VERTEX_POINT('',#10586);
#2842=VERTEX_POINT('',#10588);
#2843=VERTEX_POINT('',#10590);
#2844=VERTEX_POINT('',#10592);
#2845=VERTEX_POINT('',#10594);
#2846=VERTEX_POINT('',#10596);
#2847=VERTEX_POINT('',#10598);
#2848=VERTEX_POINT('',#10600);
#2849=VERTEX_POINT('',#10602);
#2850=VERTEX_POINT('',#10604);
#2851=VERTEX_POINT('',#10606);
#2852=VERTEX_POINT('',#10608);
#2853=VERTEX_POINT('',#10610);
#2854=VERTEX_POINT('',#10612);
#2855=VERTEX_POINT('',#10614);
#2856=VERTEX_POINT('',#10616);
#2857=VERTEX_POINT('',#10618);
#2858=VERTEX_POINT('',#10620);
#2859=VERTEX_POINT('',#10622);
#2860=VERTEX_POINT('',#10624);
#2861=VERTEX_POINT('',#10626);
#2862=VERTEX_POINT('',#10628);
#2863=VERTEX_POINT('',#10630);
#2864=VERTEX_POINT('',#10797);
#2865=VERTEX_POINT('',#10798);
#2866=VERTEX_POINT('',#10800);
#2867=VERTEX_POINT('',#10802);
#2868=VERTEX_POINT('',#10804);
#2869=VERTEX_POINT('',#10806);
#2870=VERTEX_POINT('',#10808);
#2871=VERTEX_POINT('',#10810);
#2872=VERTEX_POINT('',#10814);
#2873=VERTEX_POINT('',#10816);
#2874=VERTEX_POINT('',#10820);
#2875=VERTEX_POINT('',#10824);
#2876=VERTEX_POINT('',#10828);
#2877=VERTEX_POINT('',#10832);
#2878=VERTEX_POINT('',#10834);
#2879=VERTEX_POINT('',#10836);
#2880=VERTEX_POINT('',#10848);
#2881=VERTEX_POINT('',#10849);
#2882=VERTEX_POINT('',#10851);
#2883=VERTEX_POINT('',#10853);
#2884=VERTEX_POINT('',#10857);
#2885=VERTEX_POINT('',#10859);
#2886=VERTEX_POINT('',#10863);
#2887=VERTEX_POINT('',#10865);
#2888=VERTEX_POINT('',#10869);
#2889=VERTEX_POINT('',#10871);
#2890=VERTEX_POINT('',#10875);
#2891=VERTEX_POINT('',#10877);
#2892=VERTEX_POINT('',#10885);
#2893=VERTEX_POINT('',#10888);
#2894=VERTEX_POINT('',#10892);
#2895=VERTEX_POINT('',#10896);
#2896=EDGE_CURVE('',#2383,#2383,#2012,.T.);
#2897=EDGE_CURVE('',#2383,#2384,#1328,.T.);
#2898=EDGE_CURVE('',#2384,#2384,#2013,.T.);
#2899=EDGE_CURVE('',#2385,#2385,#2014,.T.);
#2900=EDGE_CURVE('',#2385,#2386,#1329,.T.);
#2901=EDGE_CURVE('',#2386,#2386,#2015,.T.);
#2902=EDGE_CURVE('',#2387,#2387,#2016,.T.);
#2903=EDGE_CURVE('',#2387,#2388,#1330,.T.);
#2904=EDGE_CURVE('',#2388,#2388,#2017,.T.);
#2905=EDGE_CURVE('',#2389,#2389,#2018,.T.);
#2906=EDGE_CURVE('',#2389,#2390,#1331,.T.);
#2907=EDGE_CURVE('',#2390,#2390,#2019,.T.);
#2908=EDGE_CURVE('',#2391,#2392,#1332,.T.);
#2909=EDGE_CURVE('',#2392,#2393,#1333,.T.);
#2910=EDGE_CURVE('',#2394,#2393,#1334,.T.);
#2911=EDGE_CURVE('',#2391,#2394,#1335,.T.);
#2912=EDGE_CURVE('',#2395,#2391,#1336,.T.);
#2913=EDGE_CURVE('',#2396,#2394,#1337,.T.);
#2914=EDGE_CURVE('',#2395,#2396,#1338,.T.);
#2915=EDGE_CURVE('',#2397,#2395,#1339,.T.);
#2916=EDGE_CURVE('',#2398,#2396,#1340,.T.);
#2917=EDGE_CURVE('',#2397,#2398,#1341,.T.);
#2918=EDGE_CURVE('',#2392,#2397,#1342,.T.);
#2919=EDGE_CURVE('',#2393,#2398,#1343,.T.);
#2920=EDGE_CURVE('',#2399,#2399,#2020,.T.);
#2921=EDGE_CURVE('',#2399,#2400,#1344,.T.);
#2922=EDGE_CURVE('',#2400,#2400,#2021,.T.);
#2923=EDGE_CURVE('',#2401,#2401,#2022,.T.);
#2924=EDGE_CURVE('',#2401,#2402,#1345,.T.);
#2925=EDGE_CURVE('',#2402,#2402,#2023,.T.);
#2926=EDGE_CURVE('',#2403,#2403,#2024,.T.);
#2927=EDGE_CURVE('',#2403,#2404,#1346,.T.);
#2928=EDGE_CURVE('',#2404,#2404,#2025,.T.);
#2929=EDGE_CURVE('',#2405,#2405,#2026,.T.);
#2930=EDGE_CURVE('',#2405,#2406,#1347,.T.);
#2931=EDGE_CURVE('',#2406,#2406,#2027,.T.);
#2932=EDGE_CURVE('',#2407,#2407,#2028,.T.);
#2933=EDGE_CURVE('',#2407,#2408,#1348,.T.);
#2934=EDGE_CURVE('',#2408,#2408,#2029,.T.);
#2935=EDGE_CURVE('',#2409,#2409,#2030,.T.);
#2936=EDGE_CURVE('',#2409,#2410,#1349,.T.);
#2937=EDGE_CURVE('',#2410,#2410,#2031,.T.);
#2938=EDGE_CURVE('',#2411,#2411,#2032,.T.);
#2939=EDGE_CURVE('',#2411,#2412,#1350,.T.);
#2940=EDGE_CURVE('',#2412,#2412,#2033,.T.);
#2941=EDGE_CURVE('',#2413,#2413,#2034,.T.);
#2942=EDGE_CURVE('',#2413,#2414,#1351,.T.);
#2943=EDGE_CURVE('',#2414,#2414,#2035,.T.);
#2944=EDGE_CURVE('',#2415,#2415,#2036,.T.);
#2945=EDGE_CURVE('',#2415,#2416,#1352,.T.);
#2946=EDGE_CURVE('',#2416,#2416,#2037,.T.);
#2947=EDGE_CURVE('',#2417,#2417,#2038,.T.);
#2948=EDGE_CURVE('',#2417,#2418,#1353,.T.);
#2949=EDGE_CURVE('',#2418,#2418,#2039,.T.);
#2950=EDGE_CURVE('',#2419,#2419,#2040,.T.);
#2951=EDGE_CURVE('',#2419,#2420,#1354,.T.);
#2952=EDGE_CURVE('',#2420,#2420,#2041,.T.);
#2953=EDGE_CURVE('',#2421,#2421,#2042,.T.);
#2954=EDGE_CURVE('',#2421,#2422,#1355,.T.);
#2955=EDGE_CURVE('',#2422,#2422,#2043,.T.);
#2956=EDGE_CURVE('',#2423,#2424,#2044,.T.);
#2957=EDGE_CURVE('',#2423,#2425,#1356,.T.);
#2958=EDGE_CURVE('',#2425,#2426,#1357,.T.);
#2959=EDGE_CURVE('',#2426,#2424,#1358,.T.);
#2960=EDGE_CURVE('',#2424,#2427,#2045,.T.);
#2961=EDGE_CURVE('',#2424,#2428,#1359,.T.);
#2962=EDGE_CURVE('',#2428,#2429,#1360,.T.);
#2963=EDGE_CURVE('',#2429,#2427,#1361,.T.);
#2964=EDGE_CURVE('',#2430,#2431,#2046,.T.);
#2965=EDGE_CURVE('',#2430,#2432,#1362,.T.);
#2966=EDGE_CURVE('',#2432,#2433,#1363,.T.);
#2967=EDGE_CURVE('',#2433,#2431,#1364,.T.);
#2968=EDGE_CURVE('',#2434,#2430,#2047,.T.);
#2969=EDGE_CURVE('',#2434,#2435,#1365,.T.);
#2970=EDGE_CURVE('',#2435,#2436,#1366,.T.);
#2971=EDGE_CURVE('',#2436,#2430,#1367,.T.);
#2972=EDGE_CURVE('',#2431,#2423,#1368,.T.);
#2973=EDGE_CURVE('',#2433,#2425,#1369,.T.);
#2974=EDGE_CURVE('',#2427,#2434,#1370,.T.);
#2975=EDGE_CURVE('',#2435,#2429,#1371,.T.);
#2976=EDGE_CURVE('',#2436,#2428,#1372,.T.);
#2977=EDGE_CURVE('',#2432,#2426,#1373,.T.);
#2978=EDGE_CURVE('',#2437,#2438,#2048,.T.);
#2979=EDGE_CURVE('',#2437,#2439,#1374,.T.);
#2980=EDGE_CURVE('',#2439,#2440,#1375,.T.);
#2981=EDGE_CURVE('',#2440,#2438,#1376,.T.);
#2982=EDGE_CURVE('',#2438,#2441,#2049,.T.);
#2983=EDGE_CURVE('',#2438,#2442,#1377,.T.);
#2984=EDGE_CURVE('',#2442,#2443,#1378,.T.);
#2985=EDGE_CURVE('',#2443,#2441,#1379,.T.);
#2986=EDGE_CURVE('',#2444,#2445,#2050,.T.);
#2987=EDGE_CURVE('',#2444,#2446,#1380,.T.);
#2988=EDGE_CURVE('',#2446,#2447,#1381,.T.);
#2989=EDGE_CURVE('',#2447,#2445,#1382,.T.);
#2990=EDGE_CURVE('',#2448,#2444,#2051,.T.);
#2991=EDGE_CURVE('',#2448,#2449,#1383,.T.);
#2992=EDGE_CURVE('',#2449,#2450,#1384,.T.);
#2993=EDGE_CURVE('',#2450,#2444,#1385,.T.);
#2994=EDGE_CURVE('',#2445,#2437,#1386,.T.);
#2995=EDGE_CURVE('',#2447,#2439,#1387,.T.);
#2996=EDGE_CURVE('',#2441,#2448,#1388,.T.);
#2997=EDGE_CURVE('',#2449,#2443,#1389,.T.);
#2998=EDGE_CURVE('',#2450,#2442,#1390,.T.);
#2999=EDGE_CURVE('',#2446,#2440,#1391,.T.);
#3000=EDGE_CURVE('',#2451,#2451,#2052,.T.);
#3001=EDGE_CURVE('',#2451,#2452,#1392,.T.);
#3002=EDGE_CURVE('',#2452,#2452,#2053,.T.);
#3003=EDGE_CURVE('',#2453,#2453,#2054,.T.);
#3004=EDGE_CURVE('',#2453,#2454,#1393,.T.);
#3005=EDGE_CURVE('',#2454,#2454,#2055,.T.);
#3006=EDGE_CURVE('',#2455,#2455,#2056,.T.);
#3007=EDGE_CURVE('',#2455,#2456,#1394,.T.);
#3008=EDGE_CURVE('',#2456,#2456,#2057,.T.);
#3009=EDGE_CURVE('',#2457,#2457,#2058,.T.);
#3010=EDGE_CURVE('',#2457,#2458,#1395,.T.);
#3011=EDGE_CURVE('',#2458,#2458,#2059,.T.);
#3012=EDGE_CURVE('',#2459,#2459,#2060,.T.);
#3013=EDGE_CURVE('',#2459,#2460,#1396,.T.);
#3014=EDGE_CURVE('',#2460,#2460,#2061,.T.);
#3015=EDGE_CURVE('',#2461,#2461,#2062,.T.);
#3016=EDGE_CURVE('',#2461,#2462,#1397,.T.);
#3017=EDGE_CURVE('',#2462,#2462,#2063,.T.);
#3018=EDGE_CURVE('',#2463,#2463,#2064,.T.);
#3019=EDGE_CURVE('',#2463,#2464,#1398,.T.);
#3020=EDGE_CURVE('',#2464,#2464,#2065,.T.);
#3021=EDGE_CURVE('',#2465,#2465,#2066,.T.);
#3022=EDGE_CURVE('',#2465,#2466,#1399,.T.);
#3023=EDGE_CURVE('',#2466,#2466,#2067,.T.);
#3024=EDGE_CURVE('',#2467,#2467,#2068,.T.);
#3025=EDGE_CURVE('',#2467,#2468,#1400,.T.);
#3026=EDGE_CURVE('',#2468,#2468,#2069,.T.);
#3027=EDGE_CURVE('',#2469,#2469,#2070,.T.);
#3028=EDGE_CURVE('',#2470,#2470,#2071,.T.);
#3029=EDGE_CURVE('',#2470,#2471,#1401,.T.);
#3030=EDGE_CURVE('',#2471,#2471,#2072,.T.);
#3031=EDGE_CURVE('',#2472,#2472,#2073,.T.);
#3032=EDGE_CURVE('',#2469,#2472,#1402,.T.);
#3033=EDGE_CURVE('',#2473,#2473,#2074,.T.);
#3034=EDGE_CURVE('',#2473,#2474,#1403,.T.);
#3035=EDGE_CURVE('',#2474,#2474,#2075,.T.);
#3036=EDGE_CURVE('',#2475,#2475,#2076,.T.);
#3037=EDGE_CURVE('',#2475,#2476,#1404,.T.);
#3038=EDGE_CURVE('',#2476,#2476,#2077,.T.);
#3039=EDGE_CURVE('',#2477,#2477,#2078,.T.);
#3040=EDGE_CURVE('',#2477,#2478,#1405,.T.);
#3041=EDGE_CURVE('',#2478,#2478,#2079,.T.);
#3042=EDGE_CURVE('',#2479,#2479,#2080,.T.);
#3043=EDGE_CURVE('',#2479,#2480,#1406,.T.);
#3044=EDGE_CURVE('',#2480,#2480,#2081,.T.);
#3045=EDGE_CURVE('',#2481,#2481,#2082,.T.);
#3046=EDGE_CURVE('',#2481,#2482,#1407,.T.);
#3047=EDGE_CURVE('',#2482,#2482,#2083,.T.);
#3048=EDGE_CURVE('',#2483,#2483,#2084,.T.);
#3049=EDGE_CURVE('',#2483,#2484,#1408,.T.);
#3050=EDGE_CURVE('',#2484,#2484,#2085,.T.);
#3051=EDGE_CURVE('',#2485,#2485,#2086,.T.);
#3052=EDGE_CURVE('',#2485,#2486,#1409,.T.);
#3053=EDGE_CURVE('',#2486,#2486,#2087,.T.);
#3054=EDGE_CURVE('',#2487,#2487,#2088,.T.);
#3055=EDGE_CURVE('',#2487,#2488,#1410,.T.);
#3056=EDGE_CURVE('',#2488,#2488,#2089,.T.);
#3057=EDGE_CURVE('',#2489,#2489,#2090,.T.);
#3058=EDGE_CURVE('',#2490,#2490,#2091,.T.);
#3059=EDGE_CURVE('',#2490,#2489,#1411,.T.);
#3060=EDGE_CURVE('',#2491,#2491,#2092,.T.);
#3061=EDGE_CURVE('',#2491,#2492,#1412,.T.);
#3062=EDGE_CURVE('',#2492,#2492,#2093,.T.);
#3063=EDGE_CURVE('',#2493,#2494,#1413,.T.);
#3064=EDGE_CURVE('',#2494,#2495,#1414,.T.);
#3065=EDGE_CURVE('',#2496,#2495,#1415,.T.);
#3066=EDGE_CURVE('',#2493,#2496,#1416,.T.);
#3067=EDGE_CURVE('',#2497,#2493,#1417,.T.);
#3068=EDGE_CURVE('',#2498,#2496,#1418,.T.);
#3069=EDGE_CURVE('',#2497,#2498,#1419,.T.);
#3070=EDGE_CURVE('',#2499,#2497,#1420,.T.);
#3071=EDGE_CURVE('',#2500,#2498,#1421,.T.);
#3072=EDGE_CURVE('',#2499,#2500,#1422,.T.);
#3073=EDGE_CURVE('',#2494,#2499,#1423,.T.);
#3074=EDGE_CURVE('',#2495,#2500,#1424,.T.);
#3075=EDGE_CURVE('',#2501,#2502,#1425,.T.);
#3076=EDGE_CURVE('',#2502,#2503,#1426,.T.);
#3077=EDGE_CURVE('',#2504,#2503,#1427,.T.);
#3078=EDGE_CURVE('',#2501,#2504,#1428,.T.);
#3079=EDGE_CURVE('',#2505,#2501,#1429,.T.);
#3080=EDGE_CURVE('',#2506,#2504,#1430,.T.);
#3081=EDGE_CURVE('',#2505,#2506,#1431,.T.);
#3082=EDGE_CURVE('',#2507,#2505,#1432,.T.);
#3083=EDGE_CURVE('',#2508,#2506,#1433,.T.);
#3084=EDGE_CURVE('',#2507,#2508,#1434,.T.);
#3085=EDGE_CURVE('',#2502,#2507,#1435,.T.);
#3086=EDGE_CURVE('',#2503,#2508,#1436,.T.);
#3087=EDGE_CURVE('',#2509,#2510,#2094,.T.);
#3088=EDGE_CURVE('',#2510,#2509,#2095,.T.);
#3089=EDGE_CURVE('',#2510,#2511,#2096,.T.);
#3090=EDGE_CURVE('',#2512,#2511,#2097,.T.);
#3091=EDGE_CURVE('',#2511,#2512,#2098,.T.);
#3092=EDGE_CURVE('',#2512,#2513,#1437,.T.);
#3093=EDGE_CURVE('',#2513,#2513,#2099,.T.);
#3094=EDGE_CURVE('',#2514,#2514,#2100,.T.);
#3095=EDGE_CURVE('',#2514,#2515,#1438,.T.);
#3096=EDGE_CURVE('',#2515,#2515,#2101,.T.);
#3097=EDGE_CURVE('',#2515,#2516,#1439,.T.);
#3098=EDGE_CURVE('',#2516,#2516,#2102,.T.);
#3099=EDGE_CURVE('',#2517,#2517,#2103,.T.);
#3100=EDGE_CURVE('',#2517,#2509,#1440,.T.);
#3101=EDGE_CURVE('',#2518,#2518,#2104,.T.);
#3102=EDGE_CURVE('',#2518,#2514,#1441,.T.);
#3103=EDGE_CURVE('',#2519,#2520,#2105,.T.);
#3104=EDGE_CURVE('',#2520,#2519,#2106,.T.);
#3105=EDGE_CURVE('',#2520,#2521,#2107,.T.);
#3106=EDGE_CURVE('',#2522,#2521,#2108,.T.);
#3107=EDGE_CURVE('',#2521,#2522,#2109,.T.);
#3108=EDGE_CURVE('',#2523,#2523,#2110,.T.);
#3109=EDGE_CURVE('',#2523,#2522,#1442,.T.);
#3110=EDGE_CURVE('',#2524,#2524,#2111,.T.);
#3111=EDGE_CURVE('',#2525,#2525,#2112,.T.);
#3112=EDGE_CURVE('',#2526,#2526,#2113,.T.);
#3113=EDGE_CURVE('',#2526,#2524,#1443,.T.);
#3114=EDGE_CURVE('',#2527,#2527,#2114,.T.);
#3115=EDGE_CURVE('',#2527,#2526,#1444,.T.);
#3116=EDGE_CURVE('',#2528,#2528,#2115,.T.);
#3117=EDGE_CURVE('',#2528,#2527,#1445,.T.);
#3118=EDGE_CURVE('',#2519,#2525,#1446,.T.);
#3119=EDGE_CURVE('',#2529,#2530,#2116,.T.);
#3120=EDGE_CURVE('',#2531,#2532,#2117,.T.);
#3121=EDGE_CURVE('',#2533,#2534,#2118,.T.);
#3122=EDGE_CURVE('',#2535,#2536,#2119,.T.);
#3123=EDGE_CURVE('',#2537,#2538,#2120,.T.);
#3124=EDGE_CURVE('',#2539,#2540,#2121,.T.);
#3125=EDGE_CURVE('',#2541,#2542,#2122,.T.);
#3126=EDGE_CURVE('',#2543,#2544,#2123,.T.);
#3127=EDGE_CURVE('',#2545,#2546,#163,.T.);
#3128=EDGE_CURVE('',#2547,#2545,#2124,.T.);
#3129=EDGE_CURVE('',#2548,#2547,#164,.T.);
#3130=EDGE_CURVE('',#2546,#2548,#2125,.T.);
#3131=EDGE_CURVE('',#2549,#2547,#2126,.T.);
#3132=EDGE_CURVE('',#2549,#2550,#165,.T.);
#3133=EDGE_CURVE('',#2551,#2550,#2127,.T.);
#3134=EDGE_CURVE('',#2551,#2552,#166,.T.);
#3135=EDGE_CURVE('',#2553,#2552,#2128,.T.);
#3136=EDGE_CURVE('',#2553,#2554,#167,.T.);
#3137=EDGE_CURVE('',#2554,#2555,#1447,.T.);
#3138=EDGE_CURVE('',#2555,#2555,#2129,.T.);
#3139=EDGE_CURVE('',#2554,#2556,#168,.T.);
#3140=EDGE_CURVE('',#2557,#2556,#2130,.T.);
#3141=EDGE_CURVE('',#2557,#2558,#169,.T.);
#3142=EDGE_CURVE('',#2559,#2558,#2131,.T.);
#3143=EDGE_CURVE('',#2559,#2560,#170,.T.);
#3144=EDGE_CURVE('',#2561,#2560,#2132,.T.);
#3145=EDGE_CURVE('',#2561,#2562,#171,.T.);
#3146=EDGE_CURVE('',#2563,#2562,#2133,.T.);
#3147=EDGE_CURVE('',#2563,#2564,#172,.T.);
#3148=EDGE_CURVE('',#2548,#2564,#2134,.T.);
#3149=EDGE_CURVE('',#2545,#2565,#2135,.T.);
#3150=EDGE_CURVE('',#2565,#2549,#2136,.T.);
#3151=EDGE_CURVE('',#2566,#2565,#173,.T.);
#3152=EDGE_CURVE('',#2550,#2566,#2137,.T.);
#3153=EDGE_CURVE('',#2566,#2567,#2138,.T.);
#3154=EDGE_CURVE('',#2567,#2551,#2139,.T.);
#3155=EDGE_CURVE('',#2568,#2567,#174,.T.);
#3156=EDGE_CURVE('',#2552,#2568,#2140,.T.);
#3157=EDGE_CURVE('',#2568,#2569,#2141,.T.);
#3158=EDGE_CURVE('',#2569,#2553,#2142,.T.);
#3159=EDGE_CURVE('',#2570,#2571,#175,.T.);
#3160=EDGE_CURVE('',#2556,#2570,#2143,.T.);
#3161=EDGE_CURVE('',#2571,#2569,#176,.T.);
#3162=EDGE_CURVE('',#2570,#2572,#2144,.T.);
#3163=EDGE_CURVE('',#2572,#2557,#2145,.T.);
#3164=EDGE_CURVE('',#2573,#2572,#177,.T.);
#3165=EDGE_CURVE('',#2558,#2573,#2146,.T.);
#3166=EDGE_CURVE('',#2573,#2574,#2147,.T.);
#3167=EDGE_CURVE('',#2574,#2559,#2148,.T.);
#3168=EDGE_CURVE('',#2575,#2574,#178,.T.);
#3169=EDGE_CURVE('',#2560,#2575,#2149,.T.);
#3170=EDGE_CURVE('',#2575,#2576,#2150,.T.);
#3171=EDGE_CURVE('',#2576,#2561,#2151,.T.);
#3172=EDGE_CURVE('',#2577,#2576,#179,.T.);
#3173=EDGE_CURVE('',#2562,#2577,#2152,.T.);
#3174=EDGE_CURVE('',#2578,#2578,#2153,.T.);
#3175=EDGE_CURVE('',#2578,#2571,#1448,.T.);
#3176=EDGE_CURVE('',#2579,#2546,#2154,.T.);
#3177=EDGE_CURVE('',#2579,#2580,#180,.T.);
#3178=EDGE_CURVE('',#2577,#2580,#2155,.T.);
#3179=EDGE_CURVE('',#2564,#2579,#2156,.T.);
#3180=EDGE_CURVE('',#2580,#2563,#2157,.T.);
#3181=EDGE_CURVE('',#2581,#2581,#2158,.T.);
#3182=EDGE_CURVE('',#2582,#2582,#2159,.T.);
#3183=EDGE_CURVE('',#2583,#2583,#2160,.T.);
#3184=EDGE_CURVE('',#2583,#2581,#1449,.T.);
#3185=EDGE_CURVE('',#2584,#2584,#2161,.T.);
#3186=EDGE_CURVE('',#2584,#2582,#1450,.T.);
#3187=EDGE_CURVE('',#2585,#2585,#2162,.T.);
#3188=EDGE_CURVE('',#2586,#2586,#2163,.T.);
#3189=EDGE_CURVE('',#2587,#2587,#2164,.T.);
#3190=EDGE_CURVE('',#2587,#2585,#1451,.T.);
#3191=EDGE_CURVE('',#2588,#2588,#2165,.T.);
#3192=EDGE_CURVE('',#2588,#2586,#1452,.T.);
#3193=EDGE_CURVE('',#2589,#2589,#2166,.T.);
#3194=EDGE_CURVE('',#2590,#2590,#2167,.T.);
#3195=EDGE_CURVE('',#2590,#2589,#1453,.T.);
#3196=EDGE_CURVE('',#2591,#2591,#2168,.T.);
#3197=EDGE_CURVE('',#2591,#2590,#1454,.T.);
#3198=EDGE_CURVE('',#2592,#2592,#2169,.T.);
#3199=EDGE_CURVE('',#2592,#2591,#1455,.T.);
#3200=EDGE_CURVE('',#2593,#2593,#2170,.T.);
#3201=EDGE_CURVE('',#2594,#2594,#2171,.F.);
#3202=EDGE_CURVE('',#2594,#2593,#1456,.T.);
#3203=EDGE_CURVE('',#2595,#2595,#2172,.F.);
#3204=EDGE_CURVE('',#2595,#2594,#1457,.T.);
#3205=EDGE_CURVE('',#2596,#2596,#2173,.T.);
#3206=EDGE_CURVE('',#2596,#2595,#1458,.T.);
#3207=EDGE_CURVE('',#2597,#2598,#1459,.T.);
#3208=EDGE_CURVE('',#2598,#2599,#1460,.T.);
#3209=EDGE_CURVE('',#2599,#2600,#1461,.T.);
#3210=EDGE_CURVE('',#2597,#2600,#1462,.T.);
#3211=EDGE_CURVE('',#2598,#2601,#1463,.T.);
#3212=EDGE_CURVE('',#2601,#2602,#1464,.T.);
#3213=EDGE_CURVE('',#2602,#2599,#1465,.T.);
#3214=EDGE_CURVE('',#2601,#2603,#1466,.T.);
#3215=EDGE_CURVE('',#2603,#2604,#1467,.T.);
#3216=EDGE_CURVE('',#2604,#2602,#1468,.T.);
#3217=EDGE_CURVE('',#2603,#2605,#1469,.T.);
#3218=EDGE_CURVE('',#2605,#2606,#1470,.T.);
#3219=EDGE_CURVE('',#2606,#2604,#1471,.T.);
#3220=EDGE_CURVE('',#2605,#2607,#1472,.T.);
#3221=EDGE_CURVE('',#2607,#2608,#1473,.T.);
#3222=EDGE_CURVE('',#2608,#2606,#1474,.T.);
#3223=EDGE_CURVE('',#2607,#2597,#1475,.T.);
#3224=EDGE_CURVE('',#2600,#2608,#1476,.T.);
#3225=EDGE_CURVE('',#2609,#2609,#2174,.T.);
#3226=EDGE_CURVE('',#2610,#2610,#2175,.T.);
#3227=EDGE_CURVE('',#2610,#2609,#1477,.T.);
#3228=EDGE_CURVE('',#2611,#2611,#2176,.T.);
#3229=EDGE_CURVE('',#2611,#2610,#1478,.T.);
#3230=EDGE_CURVE('',#2612,#2612,#2177,.T.);
#3231=EDGE_CURVE('',#2612,#2611,#1479,.T.);
#3232=EDGE_CURVE('',#2613,#2613,#2178,.T.);
#3233=EDGE_CURVE('',#2614,#2614,#2179,.F.);
#3234=EDGE_CURVE('',#2614,#2613,#1480,.T.);
#3235=EDGE_CURVE('',#2615,#2615,#2180,.F.);
#3236=EDGE_CURVE('',#2615,#2614,#1481,.T.);
#3237=EDGE_CURVE('',#2616,#2616,#2181,.T.);
#3238=EDGE_CURVE('',#2616,#2615,#1482,.T.);
#3239=EDGE_CURVE('',#2617,#2618,#1483,.T.);
#3240=EDGE_CURVE('',#2618,#2619,#1484,.T.);
#3241=EDGE_CURVE('',#2619,#2620,#1485,.T.);
#3242=EDGE_CURVE('',#2617,#2620,#1486,.T.);
#3243=EDGE_CURVE('',#2618,#2621,#1487,.T.);
#3244=EDGE_CURVE('',#2621,#2622,#1488,.T.);
#3245=EDGE_CURVE('',#2622,#2619,#1489,.T.);
#3246=EDGE_CURVE('',#2621,#2623,#1490,.T.);
#3247=EDGE_CURVE('',#2623,#2624,#1491,.T.);
#3248=EDGE_CURVE('',#2624,#2622,#1492,.T.);
#3249=EDGE_CURVE('',#2623,#2625,#1493,.T.);
#3250=EDGE_CURVE('',#2625,#2626,#1494,.T.);
#3251=EDGE_CURVE('',#2626,#2624,#1495,.T.);
#3252=EDGE_CURVE('',#2625,#2627,#1496,.T.);
#3253=EDGE_CURVE('',#2627,#2628,#1497,.T.);
#3254=EDGE_CURVE('',#2628,#2626,#1498,.T.);
#3255=EDGE_CURVE('',#2627,#2617,#1499,.T.);
#3256=EDGE_CURVE('',#2620,#2628,#1500,.T.);
#3257=EDGE_CURVE('',#2629,#2630,#1501,.T.);
#3258=EDGE_CURVE('',#2629,#2631,#1502,.T.);
#3259=EDGE_CURVE('',#2632,#2631,#1503,.T.);
#3260=EDGE_CURVE('',#2632,#2630,#1504,.T.);
#3261=EDGE_CURVE('',#2630,#2633,#2182,.T.);
#3262=EDGE_CURVE('',#2634,#2632,#1505,.T.);
#3263=EDGE_CURVE('',#2633,#2634,#1506,.T.);
#3264=EDGE_CURVE('',#2633,#2635,#1507,.T.);
#3265=EDGE_CURVE('',#2634,#2636,#1508,.T.);
#3266=EDGE_CURVE('',#2636,#2635,#1509,.T.);
#3267=EDGE_CURVE('',#2631,#2636,#1510,.T.);
#3268=EDGE_CURVE('',#2635,#2629,#2183,.T.);
#3269=EDGE_CURVE('',#2637,#2637,#2184,.T.);
#3270=EDGE_CURVE('',#2637,#2638,#1511,.T.);
#3271=EDGE_CURVE('',#2638,#2638,#2185,.T.);
#3272=EDGE_CURVE('',#2639,#2639,#2186,.T.);
#3273=EDGE_CURVE('',#2640,#2640,#2187,.T.);
#3274=EDGE_CURVE('',#2641,#2641,#2188,.T.);
#3275=EDGE_CURVE('',#2642,#2642,#2189,.T.);
#3276=EDGE_CURVE('',#2639,#2641,#1512,.T.);
#3277=EDGE_CURVE('',#2642,#2643,#1513,.T.);
#3278=EDGE_CURVE('',#2643,#2643,#2190,.T.);
#3279=EDGE_CURVE('',#2644,#2644,#2191,.T.);
#3280=EDGE_CURVE('',#2644,#2640,#1514,.T.);
#3281=EDGE_CURVE('',#2645,#2645,#2192,.T.);
#3282=EDGE_CURVE('',#2645,#2646,#1515,.T.);
#3283=EDGE_CURVE('',#2646,#2646,#2193,.T.);
#3284=EDGE_CURVE('',#2647,#2647,#2194,.T.);
#3285=EDGE_CURVE('',#2647,#2648,#1516,.T.);
#3286=EDGE_CURVE('',#2648,#2648,#2195,.T.);
#3287=EDGE_CURVE('',#2649,#2650,#1517,.T.);
#3288=EDGE_CURVE('',#2649,#2650,#2196,.T.);
#3289=EDGE_CURVE('',#2651,#2649,#181,.T.);
#3290=EDGE_CURVE('',#2652,#2651,#2197,.T.);
#3291=EDGE_CURVE('',#2652,#2653,#1518,.T.);
#3292=EDGE_CURVE('',#2654,#2653,#182,.T.);
#3293=EDGE_CURVE('',#2653,#2654,#183,.T.);
#3294=EDGE_CURVE('',#2655,#2652,#2198,.T.);
#3295=EDGE_CURVE('',#2650,#2655,#184,.T.);
#3296=EDGE_CURVE('',#2655,#2651,#1519,.T.);
#3297=EDGE_CURVE('',#2656,#2656,#2199,.T.);
#3298=EDGE_CURVE('',#2656,#2657,#1520,.T.);
#3299=EDGE_CURVE('',#2657,#2657,#2200,.T.);
#3300=EDGE_CURVE('',#2658,#2658,#2201,.T.);
#3301=EDGE_CURVE('',#2658,#2659,#1521,.T.);
#3302=EDGE_CURVE('',#2659,#2659,#2202,.T.);
#3303=EDGE_CURVE('',#2660,#2661,#1522,.T.);
#3304=EDGE_CURVE('',#2660,#2661,#2203,.T.);
#3305=EDGE_CURVE('',#2662,#2660,#185,.T.);
#3306=EDGE_CURVE('',#2663,#2662,#2204,.T.);
#3307=EDGE_CURVE('',#2663,#2664,#1523,.T.);
#3308=EDGE_CURVE('',#2665,#2664,#186,.T.);
#3309=EDGE_CURVE('',#2664,#2665,#187,.T.);
#3310=EDGE_CURVE('',#2666,#2663,#2205,.T.);
#3311=EDGE_CURVE('',#2661,#2666,#188,.T.);
#3312=EDGE_CURVE('',#2666,#2662,#1524,.T.);
#3313=EDGE_CURVE('',#2667,#2667,#2206,.T.);
#3314=EDGE_CURVE('',#2667,#2668,#1525,.T.);
#3315=EDGE_CURVE('',#2668,#2668,#2207,.T.);
#3316=EDGE_CURVE('',#2669,#2669,#2208,.T.);
#3317=EDGE_CURVE('',#2669,#2670,#1526,.T.);
#3318=EDGE_CURVE('',#2670,#2670,#2209,.T.);
#3319=EDGE_CURVE('',#2671,#2672,#1527,.T.);
#3320=EDGE_CURVE('',#2671,#2673,#1528,.T.);
#3321=EDGE_CURVE('',#2674,#2673,#1529,.T.);
#3322=EDGE_CURVE('',#2672,#2674,#1530,.T.);
#3323=EDGE_CURVE('',#2675,#2671,#1531,.T.);
#3324=EDGE_CURVE('',#2675,#2676,#1532,.T.);
#3325=EDGE_CURVE('',#2673,#2676,#1533,.T.);
#3326=EDGE_CURVE('',#2677,#2677,#2210,.T.);
#3327=EDGE_CURVE('',#2678,#2675,#1534,.T.);
#3328=EDGE_CURVE('',#2679,#2678,#1535,.T.);
#3329=EDGE_CURVE('',#2676,#2679,#1536,.T.);
#3330=EDGE_CURVE('',#2680,#2680,#2211,.T.);
#3331=EDGE_CURVE('',#2679,#2674,#2212,.T.);
#3332=EDGE_CURVE('',#2672,#2678,#2213,.T.);
#3333=EDGE_CURVE('',#2681,#2682,#189,.T.);
#3334=EDGE_CURVE('',#2682,#2681,#190,.T.);
#3335=EDGE_CURVE('',#2683,#2684,#191,.T.);
#3336=EDGE_CURVE('',#2684,#2683,#192,.T.);
#3337=EDGE_CURVE('',#2685,#2686,#193,.T.);
#3338=EDGE_CURVE('',#2686,#2685,#194,.T.);
#3339=EDGE_CURVE('',#2687,#2688,#195,.T.);
#3340=EDGE_CURVE('',#2689,#2687,#196,.T.);
#3341=EDGE_CURVE('',#2688,#2689,#197,.T.);
#3342=EDGE_CURVE('',#2688,#2684,#1537,.T.);
#3343=EDGE_CURVE('',#2686,#2690,#1538,.T.);
#3344=EDGE_CURVE('',#2691,#2690,#198,.T.);
#3345=EDGE_CURVE('',#2692,#2691,#199,.T.);
#3346=EDGE_CURVE('',#2690,#2692,#200,.T.);
#3347=EDGE_CURVE('',#2693,#2693,#2214,.T.);
#3348=EDGE_CURVE('',#2693,#2689,#1539,.T.);
#3349=EDGE_CURVE('',#2687,#2694,#1540,.T.);
#3350=EDGE_CURVE('',#2694,#2694,#2215,.T.);
#3351=EDGE_CURVE('',#2695,#2696,#201,.T.);
#3352=EDGE_CURVE('',#2696,#2697,#202,.T.);
#3353=EDGE_CURVE('',#2697,#2695,#203,.T.);
#3354=EDGE_CURVE('',#2698,#2699,#204,.T.);
#3355=EDGE_CURVE('',#2699,#2700,#205,.T.);
#3356=EDGE_CURVE('',#2700,#2698,#206,.T.);
#3357=EDGE_CURVE('',#2697,#2677,#1541,.T.);
#3358=EDGE_CURVE('',#2682,#2700,#1542,.T.);
#3359=EDGE_CURVE('',#2701,#2701,#2216,.T.);
#3360=EDGE_CURVE('',#2702,#2703,#2217,.T.);
#3361=EDGE_CURVE('',#2704,#2703,#2218,.T.);
#3362=EDGE_CURVE('',#2704,#2705,#2219,.T.);
#3363=EDGE_CURVE('',#2706,#2705,#2220,.T.);
#3364=EDGE_CURVE('',#2706,#2707,#2221,.T.);
#3365=EDGE_CURVE('',#2708,#2707,#2222,.T.);
#3366=EDGE_CURVE('',#2708,#2709,#2223,.T.);
#3367=EDGE_CURVE('',#2710,#2709,#2224,.T.);
#3368=EDGE_CURVE('',#2710,#2711,#2225,.T.);
#3369=EDGE_CURVE('',#2712,#2711,#2226,.T.);
#3370=EDGE_CURVE('',#2712,#2713,#2227,.T.);
#3371=EDGE_CURVE('',#2714,#2713,#2228,.T.);
#3372=EDGE_CURVE('',#2714,#2715,#2229,.T.);
#3373=EDGE_CURVE('',#2716,#2715,#2230,.T.);
#3374=EDGE_CURVE('',#2716,#2717,#2231,.T.);
#3375=EDGE_CURVE('',#2718,#2717,#2232,.T.);
#3376=EDGE_CURVE('',#2718,#2719,#2233,.T.);
#3377=EDGE_CURVE('',#2720,#2719,#2234,.T.);
#3378=EDGE_CURVE('',#2720,#2721,#2235,.T.);
#3379=EDGE_CURVE('',#2722,#2721,#2236,.T.);
#3380=EDGE_CURVE('',#2722,#2723,#2237,.T.);
#3381=EDGE_CURVE('',#2724,#2723,#2238,.T.);
#3382=EDGE_CURVE('',#2724,#2725,#2239,.T.);
#3383=EDGE_CURVE('',#2726,#2725,#2240,.T.);
#3384=EDGE_CURVE('',#2726,#2727,#2241,.T.);
#3385=EDGE_CURVE('',#2728,#2727,#2242,.T.);
#3386=EDGE_CURVE('',#2728,#2729,#2243,.T.);
#3387=EDGE_CURVE('',#2730,#2729,#2244,.T.);
#3388=EDGE_CURVE('',#2730,#2731,#2245,.T.);
#3389=EDGE_CURVE('',#2732,#2731,#2246,.T.);
#3390=EDGE_CURVE('',#2732,#2733,#2247,.T.);
#3391=EDGE_CURVE('',#2734,#2733,#2248,.T.);
#3392=EDGE_CURVE('',#2734,#2735,#2249,.T.);
#3393=EDGE_CURVE('',#2736,#2735,#2250,.T.);
#3394=EDGE_CURVE('',#2736,#2737,#2251,.T.);
#3395=EDGE_CURVE('',#2738,#2737,#2252,.T.);
#3396=EDGE_CURVE('',#2738,#2739,#2253,.T.);
#3397=EDGE_CURVE('',#2740,#2739,#2254,.T.);
#3398=EDGE_CURVE('',#2740,#2741,#2255,.T.);
#3399=EDGE_CURVE('',#2742,#2741,#2256,.T.);
#3400=EDGE_CURVE('',#2742,#2743,#2257,.T.);
#3401=EDGE_CURVE('',#2744,#2743,#2258,.T.);
#3402=EDGE_CURVE('',#2744,#2745,#2259,.T.);
#3403=EDGE_CURVE('',#2746,#2745,#2260,.T.);
#3404=EDGE_CURVE('',#2746,#2747,#2261,.T.);
#3405=EDGE_CURVE('',#2748,#2747,#2262,.T.);
#3406=EDGE_CURVE('',#2748,#2749,#2263,.T.);
#3407=EDGE_CURVE('',#2750,#2749,#2264,.T.);
#3408=EDGE_CURVE('',#2750,#2751,#2265,.T.);
#3409=EDGE_CURVE('',#2752,#2751,#2266,.T.);
#3410=EDGE_CURVE('',#2752,#2753,#2267,.T.);
#3411=EDGE_CURVE('',#2754,#2753,#2268,.T.);
#3412=EDGE_CURVE('',#2754,#2755,#2269,.T.);
#3413=EDGE_CURVE('',#2756,#2755,#2270,.T.);
#3414=EDGE_CURVE('',#2756,#2757,#2271,.T.);
#3415=EDGE_CURVE('',#2758,#2757,#2272,.T.);
#3416=EDGE_CURVE('',#2758,#2759,#2273,.T.);
#3417=EDGE_CURVE('',#2760,#2759,#2274,.T.);
#3418=EDGE_CURVE('',#2760,#2761,#2275,.T.);
#3419=EDGE_CURVE('',#2762,#2761,#2276,.T.);
#3420=EDGE_CURVE('',#2762,#2763,#2277,.T.);
#3421=EDGE_CURVE('',#2764,#2763,#2278,.T.);
#3422=EDGE_CURVE('',#2764,#2765,#2279,.T.);
#3423=EDGE_CURVE('',#2766,#2765,#2280,.T.);
#3424=EDGE_CURVE('',#2766,#2767,#2281,.T.);
#3425=EDGE_CURVE('',#2768,#2767,#2282,.T.);
#3426=EDGE_CURVE('',#2768,#2769,#2283,.T.);
#3427=EDGE_CURVE('',#2770,#2769,#2284,.T.);
#3428=EDGE_CURVE('',#2770,#2771,#2285,.T.);
#3429=EDGE_CURVE('',#2772,#2771,#2286,.T.);
#3430=EDGE_CURVE('',#2772,#2773,#2287,.T.);
#3431=EDGE_CURVE('',#2774,#2773,#2288,.T.);
#3432=EDGE_CURVE('',#2774,#2775,#2289,.T.);
#3433=EDGE_CURVE('',#2776,#2775,#2290,.T.);
#3434=EDGE_CURVE('',#2776,#2777,#2291,.T.);
#3435=EDGE_CURVE('',#2778,#2777,#2292,.T.);
#3436=EDGE_CURVE('',#2778,#2779,#2293,.T.);
#3437=EDGE_CURVE('',#2780,#2779,#2294,.T.);
#3438=EDGE_CURVE('',#2780,#2781,#2295,.T.);
#3439=EDGE_CURVE('',#2702,#2781,#2296,.T.);
#3440=EDGE_CURVE('',#2782,#2782,#2297,.T.);
#3441=EDGE_CURVE('',#2782,#2701,#1543,.T.);
#3442=EDGE_CURVE('',#2783,#2783,#2298,.T.);
#3443=EDGE_CURVE('',#2784,#2785,#2299,.T.);
#3444=EDGE_CURVE('',#2785,#2786,#2300,.T.);
#3445=EDGE_CURVE('',#2786,#2787,#2301,.T.);
#3446=EDGE_CURVE('',#2787,#2788,#2302,.T.);
#3447=EDGE_CURVE('',#2788,#2789,#2303,.T.);
#3448=EDGE_CURVE('',#2789,#2790,#2304,.T.);
#3449=EDGE_CURVE('',#2790,#2791,#2305,.T.);
#3450=EDGE_CURVE('',#2791,#2792,#2306,.T.);
#3451=EDGE_CURVE('',#2792,#2793,#2307,.T.);
#3452=EDGE_CURVE('',#2793,#2794,#2308,.T.);
#3453=EDGE_CURVE('',#2794,#2795,#2309,.T.);
#3454=EDGE_CURVE('',#2795,#2796,#2310,.T.);
#3455=EDGE_CURVE('',#2796,#2797,#2311,.T.);
#3456=EDGE_CURVE('',#2797,#2798,#2312,.T.);
#3457=EDGE_CURVE('',#2798,#2799,#2313,.T.);
#3458=EDGE_CURVE('',#2799,#2800,#2314,.T.);
#3459=EDGE_CURVE('',#2800,#2801,#2315,.T.);
#3460=EDGE_CURVE('',#2801,#2802,#2316,.T.);
#3461=EDGE_CURVE('',#2802,#2803,#2317,.T.);
#3462=EDGE_CURVE('',#2803,#2804,#2318,.T.);
#3463=EDGE_CURVE('',#2804,#2805,#2319,.T.);
#3464=EDGE_CURVE('',#2805,#2806,#2320,.T.);
#3465=EDGE_CURVE('',#2806,#2807,#2321,.T.);
#3466=EDGE_CURVE('',#2807,#2808,#2322,.T.);
#3467=EDGE_CURVE('',#2808,#2809,#2323,.T.);
#3468=EDGE_CURVE('',#2809,#2810,#2324,.T.);
#3469=EDGE_CURVE('',#2810,#2811,#2325,.T.);
#3470=EDGE_CURVE('',#2811,#2812,#2326,.T.);
#3471=EDGE_CURVE('',#2812,#2813,#2327,.T.);
#3472=EDGE_CURVE('',#2813,#2814,#2328,.T.);
#3473=EDGE_CURVE('',#2814,#2815,#2329,.T.);
#3474=EDGE_CURVE('',#2815,#2816,#2330,.T.);
#3475=EDGE_CURVE('',#2816,#2817,#2331,.T.);
#3476=EDGE_CURVE('',#2817,#2818,#2332,.T.);
#3477=EDGE_CURVE('',#2818,#2819,#2333,.T.);
#3478=EDGE_CURVE('',#2819,#2820,#2334,.T.);
#3479=EDGE_CURVE('',#2820,#2821,#2335,.T.);
#3480=EDGE_CURVE('',#2821,#2822,#2336,.T.);
#3481=EDGE_CURVE('',#2822,#2823,#2337,.T.);
#3482=EDGE_CURVE('',#2823,#2824,#2338,.T.);
#3483=EDGE_CURVE('',#2824,#2825,#2339,.T.);
#3484=EDGE_CURVE('',#2825,#2826,#2340,.T.);
#3485=EDGE_CURVE('',#2826,#2827,#2341,.T.);
#3486=EDGE_CURVE('',#2827,#2828,#2342,.T.);
#3487=EDGE_CURVE('',#2828,#2829,#2343,.T.);
#3488=EDGE_CURVE('',#2829,#2830,#2344,.T.);
#3489=EDGE_CURVE('',#2830,#2831,#2345,.T.);
#3490=EDGE_CURVE('',#2831,#2832,#2346,.T.);
#3491=EDGE_CURVE('',#2832,#2833,#2347,.T.);
#3492=EDGE_CURVE('',#2833,#2834,#2348,.T.);
#3493=EDGE_CURVE('',#2834,#2835,#2349,.T.);
#3494=EDGE_CURVE('',#2835,#2836,#2350,.T.);
#3495=EDGE_CURVE('',#2836,#2837,#2351,.T.);
#3496=EDGE_CURVE('',#2837,#2838,#2352,.T.);
#3497=EDGE_CURVE('',#2838,#2839,#2353,.T.);
#3498=EDGE_CURVE('',#2839,#2840,#2354,.T.);
#3499=EDGE_CURVE('',#2840,#2841,#2355,.T.);
#3500=EDGE_CURVE('',#2841,#2842,#2356,.T.);
#3501=EDGE_CURVE('',#2842,#2843,#2357,.T.);
#3502=EDGE_CURVE('',#2843,#2844,#2358,.T.);
#3503=EDGE_CURVE('',#2844,#2845,#2359,.T.);
#3504=EDGE_CURVE('',#2845,#2846,#2360,.T.);
#3505=EDGE_CURVE('',#2846,#2847,#2361,.T.);
#3506=EDGE_CURVE('',#2847,#2848,#2362,.T.);
#3507=EDGE_CURVE('',#2848,#2849,#2363,.T.);
#3508=EDGE_CURVE('',#2849,#2850,#2364,.T.);
#3509=EDGE_CURVE('',#2850,#2851,#2365,.T.);
#3510=EDGE_CURVE('',#2851,#2852,#2366,.T.);
#3511=EDGE_CURVE('',#2852,#2853,#2367,.T.);
#3512=EDGE_CURVE('',#2853,#2854,#2368,.T.);
#3513=EDGE_CURVE('',#2854,#2855,#2369,.T.);
#3514=EDGE_CURVE('',#2855,#2856,#2370,.T.);
#3515=EDGE_CURVE('',#2856,#2857,#2371,.T.);
#3516=EDGE_CURVE('',#2857,#2858,#2372,.T.);
#3517=EDGE_CURVE('',#2858,#2859,#2373,.T.);
#3518=EDGE_CURVE('',#2859,#2860,#2374,.T.);
#3519=EDGE_CURVE('',#2860,#2861,#2375,.T.);
#3520=EDGE_CURVE('',#2861,#2862,#2376,.T.);
#3521=EDGE_CURVE('',#2862,#2863,#2377,.T.);
#3522=EDGE_CURVE('',#2863,#2784,#2378,.T.);
#3523=EDGE_CURVE('',#2680,#2783,#1544,.T.);
#3524=EDGE_CURVE('',#2785,#2702,#1545,.T.);
#3525=EDGE_CURVE('',#2703,#2784,#1546,.T.);
#3526=EDGE_CURVE('',#2863,#2704,#1547,.T.);
#3527=EDGE_CURVE('',#2705,#2862,#1548,.T.);
#3528=EDGE_CURVE('',#2861,#2706,#1549,.T.);
#3529=EDGE_CURVE('',#2707,#2860,#1550,.T.);
#3530=EDGE_CURVE('',#2859,#2708,#1551,.T.);
#3531=EDGE_CURVE('',#2709,#2858,#1552,.T.);
#3532=EDGE_CURVE('',#2857,#2710,#1553,.T.);
#3533=EDGE_CURVE('',#2711,#2856,#1554,.T.);
#3534=EDGE_CURVE('',#2855,#2712,#1555,.T.);
#3535=EDGE_CURVE('',#2713,#2854,#1556,.T.);
#3536=EDGE_CURVE('',#2853,#2714,#1557,.T.);
#3537=EDGE_CURVE('',#2715,#2852,#1558,.T.);
#3538=EDGE_CURVE('',#2851,#2716,#1559,.T.);
#3539=EDGE_CURVE('',#2717,#2850,#1560,.T.);
#3540=EDGE_CURVE('',#2849,#2718,#1561,.T.);
#3541=EDGE_CURVE('',#2719,#2848,#1562,.T.);
#3542=EDGE_CURVE('',#2847,#2720,#1563,.T.);
#3543=EDGE_CURVE('',#2721,#2846,#1564,.T.);
#3544=EDGE_CURVE('',#2845,#2722,#1565,.T.);
#3545=EDGE_CURVE('',#2723,#2844,#1566,.T.);
#3546=EDGE_CURVE('',#2843,#2724,#1567,.T.);
#3547=EDGE_CURVE('',#2725,#2842,#1568,.T.);
#3548=EDGE_CURVE('',#2841,#2726,#1569,.T.);
#3549=EDGE_CURVE('',#2727,#2840,#1570,.T.);
#3550=EDGE_CURVE('',#2839,#2728,#1571,.T.);
#3551=EDGE_CURVE('',#2729,#2838,#1572,.T.);
#3552=EDGE_CURVE('',#2837,#2730,#1573,.T.);
#3553=EDGE_CURVE('',#2731,#2836,#1574,.T.);
#3554=EDGE_CURVE('',#2835,#2732,#1575,.T.);
#3555=EDGE_CURVE('',#2733,#2834,#1576,.T.);
#3556=EDGE_CURVE('',#2833,#2734,#1577,.T.);
#3557=EDGE_CURVE('',#2735,#2832,#1578,.T.);
#3558=EDGE_CURVE('',#2831,#2736,#1579,.T.);
#3559=EDGE_CURVE('',#2737,#2830,#1580,.T.);
#3560=EDGE_CURVE('',#2829,#2738,#1581,.T.);
#3561=EDGE_CURVE('',#2739,#2828,#1582,.T.);
#3562=EDGE_CURVE('',#2827,#2740,#1583,.T.);
#3563=EDGE_CURVE('',#2741,#2826,#1584,.T.);
#3564=EDGE_CURVE('',#2825,#2742,#1585,.T.);
#3565=EDGE_CURVE('',#2743,#2824,#1586,.T.);
#3566=EDGE_CURVE('',#2823,#2744,#1587,.T.);
#3567=EDGE_CURVE('',#2745,#2822,#1588,.T.);
#3568=EDGE_CURVE('',#2821,#2746,#1589,.T.);
#3569=EDGE_CURVE('',#2747,#2820,#1590,.T.);
#3570=EDGE_CURVE('',#2819,#2748,#1591,.T.);
#3571=EDGE_CURVE('',#2749,#2818,#1592,.T.);
#3572=EDGE_CURVE('',#2817,#2750,#1593,.T.);
#3573=EDGE_CURVE('',#2751,#2816,#1594,.T.);
#3574=EDGE_CURVE('',#2815,#2752,#1595,.T.);
#3575=EDGE_CURVE('',#2753,#2814,#1596,.T.);
#3576=EDGE_CURVE('',#2813,#2754,#1597,.T.);
#3577=EDGE_CURVE('',#2755,#2812,#1598,.T.);
#3578=EDGE_CURVE('',#2811,#2756,#1599,.T.);
#3579=EDGE_CURVE('',#2757,#2810,#1600,.T.);
#3580=EDGE_CURVE('',#2809,#2758,#1601,.T.);
#3581=EDGE_CURVE('',#2759,#2808,#1602,.T.);
#3582=EDGE_CURVE('',#2807,#2760,#1603,.T.);
#3583=EDGE_CURVE('',#2761,#2806,#1604,.T.);
#3584=EDGE_CURVE('',#2805,#2762,#1605,.T.);
#3585=EDGE_CURVE('',#2763,#2804,#1606,.T.);
#3586=EDGE_CURVE('',#2803,#2764,#1607,.T.);
#3587=EDGE_CURVE('',#2765,#2802,#1608,.T.);
#3588=EDGE_CURVE('',#2801,#2766,#1609,.T.);
#3589=EDGE_CURVE('',#2767,#2800,#1610,.T.);
#3590=EDGE_CURVE('',#2799,#2768,#1611,.T.);
#3591=EDGE_CURVE('',#2769,#2798,#1612,.T.);
#3592=EDGE_CURVE('',#2797,#2770,#1613,.T.);
#3593=EDGE_CURVE('',#2771,#2796,#1614,.T.);
#3594=EDGE_CURVE('',#2795,#2772,#1615,.T.);
#3595=EDGE_CURVE('',#2773,#2794,#1616,.T.);
#3596=EDGE_CURVE('',#2793,#2774,#1617,.T.);
#3597=EDGE_CURVE('',#2775,#2792,#1618,.T.);
#3598=EDGE_CURVE('',#2791,#2776,#1619,.T.);
#3599=EDGE_CURVE('',#2777,#2790,#1620,.T.);
#3600=EDGE_CURVE('',#2789,#2778,#1621,.T.);
#3601=EDGE_CURVE('',#2779,#2788,#1622,.T.);
#3602=EDGE_CURVE('',#2781,#2786,#1623,.T.);
#3603=EDGE_CURVE('',#2787,#2780,#1624,.T.);
#3604=EDGE_CURVE('',#2864,#2865,#1625,.T.);
#3605=EDGE_CURVE('',#2866,#2864,#1626,.T.);
#3606=EDGE_CURVE('',#2867,#2866,#1627,.T.);
#3607=EDGE_CURVE('',#2868,#2867,#1628,.T.);
#3608=EDGE_CURVE('',#2869,#2868,#1629,.T.);
#3609=EDGE_CURVE('',#2870,#2869,#1630,.T.);
#3610=EDGE_CURVE('',#2871,#2870,#1631,.T.);
#3611=EDGE_CURVE('',#2865,#2871,#1632,.T.);
#3612=EDGE_CURVE('',#2868,#2872,#1633,.T.);
#3613=EDGE_CURVE('',#2872,#2873,#1634,.T.);
#3614=EDGE_CURVE('',#2873,#2869,#1635,.T.);
#3615=EDGE_CURVE('',#2874,#2867,#1636,.T.);
#3616=EDGE_CURVE('',#2874,#2872,#1637,.T.);
#3617=EDGE_CURVE('',#2866,#2875,#1638,.T.);
#3618=EDGE_CURVE('',#2875,#2874,#1639,.T.);
#3619=EDGE_CURVE('',#2876,#2864,#1640,.T.);
#3620=EDGE_CURVE('',#2876,#2875,#1641,.T.);
#3621=EDGE_CURVE('',#2877,#2876,#1642,.T.);
#3622=EDGE_CURVE('',#2878,#2877,#1643,.T.);
#3623=EDGE_CURVE('',#2879,#2878,#1644,.T.);
#3624=EDGE_CURVE('',#2873,#2879,#1645,.T.);
#3625=EDGE_CURVE('',#2865,#2877,#1646,.T.);
#3626=EDGE_CURVE('',#2878,#2871,#1647,.T.);
#3627=EDGE_CURVE('',#2870,#2879,#1648,.T.);
#3628=EDGE_CURVE('',#2880,#2881,#1649,.T.);
#3629=EDGE_CURVE('',#2880,#2882,#1650,.T.);
#3630=EDGE_CURVE('',#2882,#2883,#1651,.T.);
#3631=EDGE_CURVE('',#2881,#2883,#1652,.T.);
#3632=EDGE_CURVE('',#2884,#2880,#1653,.T.);
#3633=EDGE_CURVE('',#2884,#2885,#1654,.T.);
#3634=EDGE_CURVE('',#2885,#2882,#1655,.T.);
#3635=EDGE_CURVE('',#2886,#2884,#1656,.T.);
#3636=EDGE_CURVE('',#2886,#2887,#1657,.T.);
#3637=EDGE_CURVE('',#2887,#2885,#1658,.T.);
#3638=EDGE_CURVE('',#2888,#2886,#1659,.T.);
#3639=EDGE_CURVE('',#2888,#2889,#1660,.T.);
#3640=EDGE_CURVE('',#2889,#2887,#1661,.T.);
#3641=EDGE_CURVE('',#2890,#2888,#1662,.T.);
#3642=EDGE_CURVE('',#2890,#2891,#1663,.T.);
#3643=EDGE_CURVE('',#2891,#2889,#1664,.T.);
#3644=EDGE_CURVE('',#2881,#2890,#1665,.T.);
#3645=EDGE_CURVE('',#2883,#2891,#1666,.T.);
#3646=EDGE_CURVE('',#2892,#2892,#2379,.T.);
#3647=EDGE_CURVE('',#2893,#2893,#2380,.T.);
#3648=EDGE_CURVE('',#2893,#2892,#1667,.T.);
#3649=EDGE_CURVE('',#2894,#2894,#2381,.F.);
#3650=EDGE_CURVE('',#2894,#2893,#1668,.T.);
#3651=EDGE_CURVE('',#2895,#2895,#2382,.T.);
#3652=EDGE_CURVE('',#2895,#2894,#1669,.T.);
#3653=ORIENTED_EDGE('',*,*,#2896,.F.);
#3654=ORIENTED_EDGE('',*,*,#2897,.T.);
#3655=ORIENTED_EDGE('',*,*,#2898,.F.);
#3656=ORIENTED_EDGE('',*,*,#2897,.F.);
#3657=ORIENTED_EDGE('',*,*,#2899,.F.);
#3658=ORIENTED_EDGE('',*,*,#2900,.T.);
#3659=ORIENTED_EDGE('',*,*,#2901,.F.);
#3660=ORIENTED_EDGE('',*,*,#2900,.F.);
#3661=ORIENTED_EDGE('',*,*,#2902,.F.);
#3662=ORIENTED_EDGE('',*,*,#2903,.T.);
#3663=ORIENTED_EDGE('',*,*,#2904,.F.);
#3664=ORIENTED_EDGE('',*,*,#2903,.F.);
#3665=ORIENTED_EDGE('',*,*,#2905,.F.);
#3666=ORIENTED_EDGE('',*,*,#2906,.T.);
#3667=ORIENTED_EDGE('',*,*,#2907,.F.);
#3668=ORIENTED_EDGE('',*,*,#2906,.F.);
#3669=ORIENTED_EDGE('',*,*,#2908,.T.);
#3670=ORIENTED_EDGE('',*,*,#2909,.T.);
#3671=ORIENTED_EDGE('',*,*,#2910,.F.);
#3672=ORIENTED_EDGE('',*,*,#2911,.F.);
#3673=ORIENTED_EDGE('',*,*,#2912,.T.);
#3674=ORIENTED_EDGE('',*,*,#2911,.T.);
#3675=ORIENTED_EDGE('',*,*,#2913,.F.);
#3676=ORIENTED_EDGE('',*,*,#2914,.F.);
#3677=ORIENTED_EDGE('',*,*,#2915,.T.);
#3678=ORIENTED_EDGE('',*,*,#2914,.T.);
#3679=ORIENTED_EDGE('',*,*,#2916,.F.);
#3680=ORIENTED_EDGE('',*,*,#2917,.F.);
#3681=ORIENTED_EDGE('',*,*,#2918,.T.);
#3682=ORIENTED_EDGE('',*,*,#2917,.T.);
#3683=ORIENTED_EDGE('',*,*,#2919,.F.);
#3684=ORIENTED_EDGE('',*,*,#2909,.F.);
#3685=ORIENTED_EDGE('',*,*,#2919,.T.);
#3686=ORIENTED_EDGE('',*,*,#2916,.T.);
#3687=ORIENTED_EDGE('',*,*,#2913,.T.);
#3688=ORIENTED_EDGE('',*,*,#2910,.T.);
#3689=ORIENTED_EDGE('',*,*,#2898,.T.);
#3690=ORIENTED_EDGE('',*,*,#2901,.T.);
#3691=ORIENTED_EDGE('',*,*,#2904,.T.);
#3692=ORIENTED_EDGE('',*,*,#2907,.T.);
#3693=ORIENTED_EDGE('',*,*,#2918,.F.);
#3694=ORIENTED_EDGE('',*,*,#2908,.F.);
#3695=ORIENTED_EDGE('',*,*,#2912,.F.);
#3696=ORIENTED_EDGE('',*,*,#2915,.F.);
#3697=ORIENTED_EDGE('',*,*,#2896,.T.);
#3698=ORIENTED_EDGE('',*,*,#2899,.T.);
#3699=ORIENTED_EDGE('',*,*,#2902,.T.);
#3700=ORIENTED_EDGE('',*,*,#2905,.T.);
#3701=ORIENTED_EDGE('',*,*,#2920,.F.);
#3702=ORIENTED_EDGE('',*,*,#2921,.T.);
#3703=ORIENTED_EDGE('',*,*,#2922,.F.);
#3704=ORIENTED_EDGE('',*,*,#2921,.F.);
#3705=ORIENTED_EDGE('',*,*,#2920,.T.);
#3706=ORIENTED_EDGE('',*,*,#2923,.F.);
#3707=ORIENTED_EDGE('',*,*,#2924,.T.);
#3708=ORIENTED_EDGE('',*,*,#2925,.F.);
#3709=ORIENTED_EDGE('',*,*,#2924,.F.);
#3710=ORIENTED_EDGE('',*,*,#2923,.T.);
#3711=ORIENTED_EDGE('',*,*,#2926,.F.);
#3712=ORIENTED_EDGE('',*,*,#2927,.T.);
#3713=ORIENTED_EDGE('',*,*,#2928,.F.);
#3714=ORIENTED_EDGE('',*,*,#2927,.F.);
#3715=ORIENTED_EDGE('',*,*,#2926,.T.);
#3716=ORIENTED_EDGE('',*,*,#2929,.F.);
#3717=ORIENTED_EDGE('',*,*,#2930,.T.);
#3718=ORIENTED_EDGE('',*,*,#2931,.F.);
#3719=ORIENTED_EDGE('',*,*,#2930,.F.);
#3720=ORIENTED_EDGE('',*,*,#2929,.T.);
#3721=ORIENTED_EDGE('',*,*,#2932,.F.);
#3722=ORIENTED_EDGE('',*,*,#2933,.T.);
#3723=ORIENTED_EDGE('',*,*,#2934,.T.);
#3724=ORIENTED_EDGE('',*,*,#2933,.F.);
#3725=ORIENTED_EDGE('',*,*,#2934,.F.);
#3726=ORIENTED_EDGE('',*,*,#2935,.F.);
#3727=ORIENTED_EDGE('',*,*,#2936,.T.);
#3728=ORIENTED_EDGE('',*,*,#2937,.T.);
#3729=ORIENTED_EDGE('',*,*,#2936,.F.);
#3730=ORIENTED_EDGE('',*,*,#2937,.F.);
#3731=ORIENTED_EDGE('',*,*,#2938,.F.);
#3732=ORIENTED_EDGE('',*,*,#2939,.T.);
#3733=ORIENTED_EDGE('',*,*,#2940,.T.);
#3734=ORIENTED_EDGE('',*,*,#2939,.F.);
#3735=ORIENTED_EDGE('',*,*,#2940,.F.);
#3736=ORIENTED_EDGE('',*,*,#2941,.F.);
#3737=ORIENTED_EDGE('',*,*,#2942,.T.);
#3738=ORIENTED_EDGE('',*,*,#2943,.T.);
#3739=ORIENTED_EDGE('',*,*,#2942,.F.);
#3740=ORIENTED_EDGE('',*,*,#2943,.F.);
#3741=ORIENTED_EDGE('',*,*,#2944,.F.);
#3742=ORIENTED_EDGE('',*,*,#2945,.T.);
#3743=ORIENTED_EDGE('',*,*,#2946,.F.);
#3744=ORIENTED_EDGE('',*,*,#2945,.F.);
#3745=ORIENTED_EDGE('',*,*,#2947,.F.);
#3746=ORIENTED_EDGE('',*,*,#2948,.T.);
#3747=ORIENTED_EDGE('',*,*,#2949,.F.);
#3748=ORIENTED_EDGE('',*,*,#2948,.F.);
#3749=ORIENTED_EDGE('',*,*,#2950,.F.);
#3750=ORIENTED_EDGE('',*,*,#2951,.T.);
#3751=ORIENTED_EDGE('',*,*,#2952,.F.);
#3752=ORIENTED_EDGE('',*,*,#2951,.F.);
#3753=ORIENTED_EDGE('',*,*,#2953,.F.);
#3754=ORIENTED_EDGE('',*,*,#2954,.T.);
#3755=ORIENTED_EDGE('',*,*,#2955,.F.);
#3756=ORIENTED_EDGE('',*,*,#2954,.F.);
#3757=ORIENTED_EDGE('',*,*,#2956,.F.);
#3758=ORIENTED_EDGE('',*,*,#2957,.T.);
#3759=ORIENTED_EDGE('',*,*,#2958,.T.);
#3760=ORIENTED_EDGE('',*,*,#2959,.T.);
#3761=ORIENTED_EDGE('',*,*,#2960,.F.);
#3762=ORIENTED_EDGE('',*,*,#2961,.T.);
#3763=ORIENTED_EDGE('',*,*,#2962,.T.);
#3764=ORIENTED_EDGE('',*,*,#2963,.T.);
#3765=ORIENTED_EDGE('',*,*,#2964,.F.);
#3766=ORIENTED_EDGE('',*,*,#2965,.T.);
#3767=ORIENTED_EDGE('',*,*,#2966,.T.);
#3768=ORIENTED_EDGE('',*,*,#2967,.T.);
#3769=ORIENTED_EDGE('',*,*,#2968,.F.);
#3770=ORIENTED_EDGE('',*,*,#2969,.T.);
#3771=ORIENTED_EDGE('',*,*,#2970,.T.);
#3772=ORIENTED_EDGE('',*,*,#2971,.T.);
#3773=ORIENTED_EDGE('',*,*,#2972,.F.);
#3774=ORIENTED_EDGE('',*,*,#2967,.F.);
#3775=ORIENTED_EDGE('',*,*,#2973,.T.);
#3776=ORIENTED_EDGE('',*,*,#2957,.F.);
#3777=ORIENTED_EDGE('',*,*,#2955,.T.);
#3778=ORIENTED_EDGE('',*,*,#2974,.F.);
#3779=ORIENTED_EDGE('',*,*,#2963,.F.);
#3780=ORIENTED_EDGE('',*,*,#2975,.F.);
#3781=ORIENTED_EDGE('',*,*,#2969,.F.);
#3782=ORIENTED_EDGE('',*,*,#2949,.T.);
#3783=ORIENTED_EDGE('',*,*,#2970,.F.);
#3784=ORIENTED_EDGE('',*,*,#2975,.T.);
#3785=ORIENTED_EDGE('',*,*,#2962,.F.);
#3786=ORIENTED_EDGE('',*,*,#2976,.F.);
#3787=ORIENTED_EDGE('',*,*,#2959,.F.);
#3788=ORIENTED_EDGE('',*,*,#2977,.F.);
#3789=ORIENTED_EDGE('',*,*,#2965,.F.);
#3790=ORIENTED_EDGE('',*,*,#2971,.F.);
#3791=ORIENTED_EDGE('',*,*,#2976,.T.);
#3792=ORIENTED_EDGE('',*,*,#2961,.F.);
#3793=ORIENTED_EDGE('',*,*,#2947,.T.);
#3794=ORIENTED_EDGE('',*,*,#2953,.T.);
#3795=ORIENTED_EDGE('',*,*,#2966,.F.);
#3796=ORIENTED_EDGE('',*,*,#2977,.T.);
#3797=ORIENTED_EDGE('',*,*,#2958,.F.);
#3798=ORIENTED_EDGE('',*,*,#2973,.F.);
#3799=ORIENTED_EDGE('',*,*,#2978,.F.);
#3800=ORIENTED_EDGE('',*,*,#2979,.T.);
#3801=ORIENTED_EDGE('',*,*,#2980,.T.);
#3802=ORIENTED_EDGE('',*,*,#2981,.T.);
#3803=ORIENTED_EDGE('',*,*,#2982,.F.);
#3804=ORIENTED_EDGE('',*,*,#2983,.T.);
#3805=ORIENTED_EDGE('',*,*,#2984,.T.);
#3806=ORIENTED_EDGE('',*,*,#2985,.T.);
#3807=ORIENTED_EDGE('',*,*,#2986,.F.);
#3808=ORIENTED_EDGE('',*,*,#2987,.T.);
#3809=ORIENTED_EDGE('',*,*,#2988,.T.);
#3810=ORIENTED_EDGE('',*,*,#2989,.T.);
#3811=ORIENTED_EDGE('',*,*,#2990,.F.);
#3812=ORIENTED_EDGE('',*,*,#2991,.T.);
#3813=ORIENTED_EDGE('',*,*,#2992,.T.);
#3814=ORIENTED_EDGE('',*,*,#2993,.T.);
#3815=ORIENTED_EDGE('',*,*,#2994,.F.);
#3816=ORIENTED_EDGE('',*,*,#2989,.F.);
#3817=ORIENTED_EDGE('',*,*,#2995,.T.);
#3818=ORIENTED_EDGE('',*,*,#2979,.F.);
#3819=ORIENTED_EDGE('',*,*,#2946,.T.);
#3820=ORIENTED_EDGE('',*,*,#2996,.F.);
#3821=ORIENTED_EDGE('',*,*,#2985,.F.);
#3822=ORIENTED_EDGE('',*,*,#2997,.F.);
#3823=ORIENTED_EDGE('',*,*,#2991,.F.);
#3824=ORIENTED_EDGE('',*,*,#2952,.T.);
#3825=ORIENTED_EDGE('',*,*,#2992,.F.);
#3826=ORIENTED_EDGE('',*,*,#2997,.T.);
#3827=ORIENTED_EDGE('',*,*,#2984,.F.);
#3828=ORIENTED_EDGE('',*,*,#2998,.F.);
#3829=ORIENTED_EDGE('',*,*,#2981,.F.);
#3830=ORIENTED_EDGE('',*,*,#2999,.F.);
#3831=ORIENTED_EDGE('',*,*,#2987,.F.);
#3832=ORIENTED_EDGE('',*,*,#2993,.F.);
#3833=ORIENTED_EDGE('',*,*,#2998,.T.);
#3834=ORIENTED_EDGE('',*,*,#2983,.F.);
#3835=ORIENTED_EDGE('',*,*,#2944,.T.);
#3836=ORIENTED_EDGE('',*,*,#2950,.T.);
#3837=ORIENTED_EDGE('',*,*,#2988,.F.);
#3838=ORIENTED_EDGE('',*,*,#2999,.T.);
#3839=ORIENTED_EDGE('',*,*,#2980,.F.);
#3840=ORIENTED_EDGE('',*,*,#2995,.F.);
#3841=ORIENTED_EDGE('',*,*,#3000,.F.);
#3842=ORIENTED_EDGE('',*,*,#3001,.T.);
#3843=ORIENTED_EDGE('',*,*,#3002,.T.);
#3844=ORIENTED_EDGE('',*,*,#3001,.F.);
#3845=ORIENTED_EDGE('',*,*,#3003,.F.);
#3846=ORIENTED_EDGE('',*,*,#3004,.T.);
#3847=ORIENTED_EDGE('',*,*,#3005,.T.);
#3848=ORIENTED_EDGE('',*,*,#3004,.F.);
#3849=ORIENTED_EDGE('',*,*,#2972,.T.);
#3850=ORIENTED_EDGE('',*,*,#2956,.T.);
#3851=ORIENTED_EDGE('',*,*,#2960,.T.);
#3852=ORIENTED_EDGE('',*,*,#2974,.T.);
#3853=ORIENTED_EDGE('',*,*,#2968,.T.);
#3854=ORIENTED_EDGE('',*,*,#2964,.T.);
#3855=ORIENTED_EDGE('',*,*,#2994,.T.);
#3856=ORIENTED_EDGE('',*,*,#2978,.T.);
#3857=ORIENTED_EDGE('',*,*,#2982,.T.);
#3858=ORIENTED_EDGE('',*,*,#2996,.T.);
#3859=ORIENTED_EDGE('',*,*,#2990,.T.);
#3860=ORIENTED_EDGE('',*,*,#2986,.T.);
#3861=ORIENTED_EDGE('',*,*,#3003,.T.);
#3862=ORIENTED_EDGE('',*,*,#3000,.T.);
#3863=ORIENTED_EDGE('',*,*,#2931,.T.);
#3864=ORIENTED_EDGE('',*,*,#2928,.T.);
#3865=ORIENTED_EDGE('',*,*,#2925,.T.);
#3866=ORIENTED_EDGE('',*,*,#2922,.T.);
#3867=ORIENTED_EDGE('',*,*,#3005,.F.);
#3868=ORIENTED_EDGE('',*,*,#3002,.F.);
#3869=ORIENTED_EDGE('',*,*,#2941,.T.);
#3870=ORIENTED_EDGE('',*,*,#2938,.T.);
#3871=ORIENTED_EDGE('',*,*,#2935,.T.);
#3872=ORIENTED_EDGE('',*,*,#2932,.T.);
#3873=ORIENTED_EDGE('',*,*,#3006,.F.);
#3874=ORIENTED_EDGE('',*,*,#3007,.T.);
#3875=ORIENTED_EDGE('',*,*,#3008,.T.);
#3876=ORIENTED_EDGE('',*,*,#3007,.F.);
#3877=ORIENTED_EDGE('',*,*,#3009,.F.);
#3878=ORIENTED_EDGE('',*,*,#3010,.T.);
#3879=ORIENTED_EDGE('',*,*,#3011,.T.);
#3880=ORIENTED_EDGE('',*,*,#3010,.F.);
#3881=ORIENTED_EDGE('',*,*,#3009,.T.);
#3882=ORIENTED_EDGE('',*,*,#3006,.T.);
#3883=ORIENTED_EDGE('',*,*,#3011,.F.);
#3884=ORIENTED_EDGE('',*,*,#3008,.F.);
#3885=ORIENTED_EDGE('',*,*,#3012,.F.);
#3886=ORIENTED_EDGE('',*,*,#3013,.T.);
#3887=ORIENTED_EDGE('',*,*,#3014,.F.);
#3888=ORIENTED_EDGE('',*,*,#3013,.F.);
#3889=ORIENTED_EDGE('',*,*,#3015,.F.);
#3890=ORIENTED_EDGE('',*,*,#3016,.T.);
#3891=ORIENTED_EDGE('',*,*,#3017,.F.);
#3892=ORIENTED_EDGE('',*,*,#3016,.F.);
#3893=ORIENTED_EDGE('',*,*,#3018,.F.);
#3894=ORIENTED_EDGE('',*,*,#3019,.T.);
#3895=ORIENTED_EDGE('',*,*,#3020,.F.);
#3896=ORIENTED_EDGE('',*,*,#3019,.F.);
#3897=ORIENTED_EDGE('',*,*,#3021,.F.);
#3898=ORIENTED_EDGE('',*,*,#3022,.T.);
#3899=ORIENTED_EDGE('',*,*,#3023,.F.);
#3900=ORIENTED_EDGE('',*,*,#3022,.F.);
#3901=ORIENTED_EDGE('',*,*,#3024,.F.);
#3902=ORIENTED_EDGE('',*,*,#3025,.T.);
#3903=ORIENTED_EDGE('',*,*,#3026,.F.);
#3904=ORIENTED_EDGE('',*,*,#3025,.F.);
#3905=ORIENTED_EDGE('',*,*,#3024,.T.);
#3906=ORIENTED_EDGE('',*,*,#3027,.T.);
#3907=ORIENTED_EDGE('',*,*,#3028,.F.);
#3908=ORIENTED_EDGE('',*,*,#3029,.T.);
#3909=ORIENTED_EDGE('',*,*,#3030,.T.);
#3910=ORIENTED_EDGE('',*,*,#3029,.F.);
#3911=ORIENTED_EDGE('',*,*,#3030,.F.);
#3912=ORIENTED_EDGE('',*,*,#3031,.F.);
#3913=ORIENTED_EDGE('',*,*,#3027,.F.);
#3914=ORIENTED_EDGE('',*,*,#3032,.T.);
#3915=ORIENTED_EDGE('',*,*,#3031,.T.);
#3916=ORIENTED_EDGE('',*,*,#3032,.F.);
#3917=ORIENTED_EDGE('',*,*,#3033,.F.);
#3918=ORIENTED_EDGE('',*,*,#3034,.T.);
#3919=ORIENTED_EDGE('',*,*,#3035,.T.);
#3920=ORIENTED_EDGE('',*,*,#3034,.F.);
#3921=ORIENTED_EDGE('',*,*,#3033,.T.);
#3922=ORIENTED_EDGE('',*,*,#3026,.T.);
#3923=ORIENTED_EDGE('',*,*,#3023,.T.);
#3924=ORIENTED_EDGE('',*,*,#3020,.T.);
#3925=ORIENTED_EDGE('',*,*,#3017,.T.);
#3926=ORIENTED_EDGE('',*,*,#3014,.T.);
#3927=ORIENTED_EDGE('',*,*,#3035,.F.);
#3928=ORIENTED_EDGE('',*,*,#3028,.T.);
#3929=ORIENTED_EDGE('',*,*,#3021,.T.);
#3930=ORIENTED_EDGE('',*,*,#3018,.T.);
#3931=ORIENTED_EDGE('',*,*,#3015,.T.);
#3932=ORIENTED_EDGE('',*,*,#3012,.T.);
#3933=ORIENTED_EDGE('',*,*,#3036,.F.);
#3934=ORIENTED_EDGE('',*,*,#3037,.T.);
#3935=ORIENTED_EDGE('',*,*,#3038,.T.);
#3936=ORIENTED_EDGE('',*,*,#3037,.F.);
#3937=ORIENTED_EDGE('',*,*,#3039,.F.);
#3938=ORIENTED_EDGE('',*,*,#3040,.T.);
#3939=ORIENTED_EDGE('',*,*,#3041,.T.);
#3940=ORIENTED_EDGE('',*,*,#3040,.F.);
#3941=ORIENTED_EDGE('',*,*,#3039,.T.);
#3942=ORIENTED_EDGE('',*,*,#3036,.T.);
#3943=ORIENTED_EDGE('',*,*,#3041,.F.);
#3944=ORIENTED_EDGE('',*,*,#3038,.F.);
#3945=ORIENTED_EDGE('',*,*,#3042,.F.);
#3946=ORIENTED_EDGE('',*,*,#3043,.T.);
#3947=ORIENTED_EDGE('',*,*,#3044,.F.);
#3948=ORIENTED_EDGE('',*,*,#3043,.F.);
#3949=ORIENTED_EDGE('',*,*,#3045,.F.);
#3950=ORIENTED_EDGE('',*,*,#3046,.T.);
#3951=ORIENTED_EDGE('',*,*,#3047,.F.);
#3952=ORIENTED_EDGE('',*,*,#3046,.F.);
#3953=ORIENTED_EDGE('',*,*,#3048,.F.);
#3954=ORIENTED_EDGE('',*,*,#3049,.T.);
#3955=ORIENTED_EDGE('',*,*,#3050,.F.);
#3956=ORIENTED_EDGE('',*,*,#3049,.F.);
#3957=ORIENTED_EDGE('',*,*,#3051,.F.);
#3958=ORIENTED_EDGE('',*,*,#3052,.T.);
#3959=ORIENTED_EDGE('',*,*,#3053,.F.);
#3960=ORIENTED_EDGE('',*,*,#3052,.F.);
#3961=ORIENTED_EDGE('',*,*,#3054,.F.);
#3962=ORIENTED_EDGE('',*,*,#3055,.T.);
#3963=ORIENTED_EDGE('',*,*,#3056,.T.);
#3964=ORIENTED_EDGE('',*,*,#3055,.F.);
#3965=ORIENTED_EDGE('',*,*,#3056,.F.);
#3966=ORIENTED_EDGE('',*,*,#3057,.F.);
#3967=ORIENTED_EDGE('',*,*,#3058,.F.);
#3968=ORIENTED_EDGE('',*,*,#3059,.T.);
#3969=ORIENTED_EDGE('',*,*,#3057,.T.);
#3970=ORIENTED_EDGE('',*,*,#3059,.F.);
#3971=ORIENTED_EDGE('',*,*,#3060,.F.);
#3972=ORIENTED_EDGE('',*,*,#3061,.T.);
#3973=ORIENTED_EDGE('',*,*,#3062,.T.);
#3974=ORIENTED_EDGE('',*,*,#3061,.F.);
#3975=ORIENTED_EDGE('',*,*,#3060,.T.);
#3976=ORIENTED_EDGE('',*,*,#3058,.T.);
#3977=ORIENTED_EDGE('',*,*,#3053,.T.);
#3978=ORIENTED_EDGE('',*,*,#3050,.T.);
#3979=ORIENTED_EDGE('',*,*,#3047,.T.);
#3980=ORIENTED_EDGE('',*,*,#3044,.T.);
#3981=ORIENTED_EDGE('',*,*,#3062,.F.);
#3982=ORIENTED_EDGE('',*,*,#3054,.T.);
#3983=ORIENTED_EDGE('',*,*,#3051,.T.);
#3984=ORIENTED_EDGE('',*,*,#3048,.T.);
#3985=ORIENTED_EDGE('',*,*,#3045,.T.);
#3986=ORIENTED_EDGE('',*,*,#3042,.T.);
#3987=ORIENTED_EDGE('',*,*,#3063,.T.);
#3988=ORIENTED_EDGE('',*,*,#3064,.T.);
#3989=ORIENTED_EDGE('',*,*,#3065,.F.);
#3990=ORIENTED_EDGE('',*,*,#3066,.F.);
#3991=ORIENTED_EDGE('',*,*,#3067,.T.);
#3992=ORIENTED_EDGE('',*,*,#3066,.T.);
#3993=ORIENTED_EDGE('',*,*,#3068,.F.);
#3994=ORIENTED_EDGE('',*,*,#3069,.F.);
#3995=ORIENTED_EDGE('',*,*,#3070,.T.);
#3996=ORIENTED_EDGE('',*,*,#3069,.T.);
#3997=ORIENTED_EDGE('',*,*,#3071,.F.);
#3998=ORIENTED_EDGE('',*,*,#3072,.F.);
#3999=ORIENTED_EDGE('',*,*,#3073,.T.);
#4000=ORIENTED_EDGE('',*,*,#3072,.T.);
#4001=ORIENTED_EDGE('',*,*,#3074,.F.);
#4002=ORIENTED_EDGE('',*,*,#3064,.F.);
#4003=ORIENTED_EDGE('',*,*,#3074,.T.);
#4004=ORIENTED_EDGE('',*,*,#3071,.T.);
#4005=ORIENTED_EDGE('',*,*,#3068,.T.);
#4006=ORIENTED_EDGE('',*,*,#3065,.T.);
#4007=ORIENTED_EDGE('',*,*,#3073,.F.);
#4008=ORIENTED_EDGE('',*,*,#3063,.F.);
#4009=ORIENTED_EDGE('',*,*,#3067,.F.);
#4010=ORIENTED_EDGE('',*,*,#3070,.F.);
#4011=ORIENTED_EDGE('',*,*,#3075,.T.);
#4012=ORIENTED_EDGE('',*,*,#3076,.T.);
#4013=ORIENTED_EDGE('',*,*,#3077,.F.);
#4014=ORIENTED_EDGE('',*,*,#3078,.F.);
#4015=ORIENTED_EDGE('',*,*,#3079,.T.);
#4016=ORIENTED_EDGE('',*,*,#3078,.T.);
#4017=ORIENTED_EDGE('',*,*,#3080,.F.);
#4018=ORIENTED_EDGE('',*,*,#3081,.F.);
#4019=ORIENTED_EDGE('',*,*,#3082,.T.);
#4020=ORIENTED_EDGE('',*,*,#3081,.T.);
#4021=ORIENTED_EDGE('',*,*,#3083,.F.);
#4022=ORIENTED_EDGE('',*,*,#3084,.F.);
#4023=ORIENTED_EDGE('',*,*,#3085,.T.);
#4024=ORIENTED_EDGE('',*,*,#3084,.T.);
#4025=ORIENTED_EDGE('',*,*,#3086,.F.);
#4026=ORIENTED_EDGE('',*,*,#3076,.F.);
#4027=ORIENTED_EDGE('',*,*,#3086,.T.);
#4028=ORIENTED_EDGE('',*,*,#3083,.T.);
#4029=ORIENTED_EDGE('',*,*,#3080,.T.);
#4030=ORIENTED_EDGE('',*,*,#3077,.T.);
#4031=ORIENTED_EDGE('',*,*,#3085,.F.);
#4032=ORIENTED_EDGE('',*,*,#3075,.F.);
#4033=ORIENTED_EDGE('',*,*,#3079,.F.);
#4034=ORIENTED_EDGE('',*,*,#3082,.F.);
#4035=ORIENTED_EDGE('',*,*,#3087,.F.);
#4036=ORIENTED_EDGE('',*,*,#3088,.F.);
#4037=ORIENTED_EDGE('',*,*,#3089,.T.);
#4038=ORIENTED_EDGE('',*,*,#3090,.F.);
#4039=ORIENTED_EDGE('',*,*,#3091,.F.);
#4040=ORIENTED_EDGE('',*,*,#3089,.F.);
#4041=ORIENTED_EDGE('',*,*,#3090,.T.);
#4042=ORIENTED_EDGE('',*,*,#3091,.T.);
#4043=ORIENTED_EDGE('',*,*,#3092,.T.);
#4044=ORIENTED_EDGE('',*,*,#3093,.T.);
#4045=ORIENTED_EDGE('',*,*,#3092,.F.);
#4046=ORIENTED_EDGE('',*,*,#3094,.T.);
#4047=ORIENTED_EDGE('',*,*,#3095,.T.);
#4048=ORIENTED_EDGE('',*,*,#3096,.F.);
#4049=ORIENTED_EDGE('',*,*,#3095,.F.);
#4050=ORIENTED_EDGE('',*,*,#3096,.T.);
#4051=ORIENTED_EDGE('',*,*,#3097,.T.);
#4052=ORIENTED_EDGE('',*,*,#3098,.F.);
#4053=ORIENTED_EDGE('',*,*,#3097,.F.);
#4054=ORIENTED_EDGE('',*,*,#3093,.F.);
#4055=ORIENTED_EDGE('',*,*,#3098,.T.);
#4056=ORIENTED_EDGE('',*,*,#3099,.F.);
#4057=ORIENTED_EDGE('',*,*,#3100,.T.);
#4058=ORIENTED_EDGE('',*,*,#3087,.T.);
#4059=ORIENTED_EDGE('',*,*,#3088,.T.);
#4060=ORIENTED_EDGE('',*,*,#3100,.F.);
#4061=ORIENTED_EDGE('',*,*,#3099,.T.);
#4062=ORIENTED_EDGE('',*,*,#3101,.F.);
#4063=ORIENTED_EDGE('',*,*,#3101,.T.);
#4064=ORIENTED_EDGE('',*,*,#3102,.T.);
#4065=ORIENTED_EDGE('',*,*,#3094,.F.);
#4066=ORIENTED_EDGE('',*,*,#3102,.F.);
#4067=ORIENTED_EDGE('',*,*,#3103,.F.);
#4068=ORIENTED_EDGE('',*,*,#3104,.F.);
#4069=ORIENTED_EDGE('',*,*,#3105,.T.);
#4070=ORIENTED_EDGE('',*,*,#3106,.F.);
#4071=ORIENTED_EDGE('',*,*,#3107,.F.);
#4072=ORIENTED_EDGE('',*,*,#3105,.F.);
#4073=ORIENTED_EDGE('',*,*,#3108,.T.);
#4074=ORIENTED_EDGE('',*,*,#3109,.T.);
#4075=ORIENTED_EDGE('',*,*,#3106,.T.);
#4076=ORIENTED_EDGE('',*,*,#3107,.T.);
#4077=ORIENTED_EDGE('',*,*,#3109,.F.);
#4078=ORIENTED_EDGE('',*,*,#3110,.F.);
#4079=ORIENTED_EDGE('',*,*,#3111,.T.);
#4080=ORIENTED_EDGE('',*,*,#3112,.F.);
#4081=ORIENTED_EDGE('',*,*,#3113,.T.);
#4082=ORIENTED_EDGE('',*,*,#3110,.T.);
#4083=ORIENTED_EDGE('',*,*,#3113,.F.);
#4084=ORIENTED_EDGE('',*,*,#3114,.F.);
#4085=ORIENTED_EDGE('',*,*,#3115,.T.);
#4086=ORIENTED_EDGE('',*,*,#3112,.T.);
#4087=ORIENTED_EDGE('',*,*,#3115,.F.);
#4088=ORIENTED_EDGE('',*,*,#3116,.F.);
#4089=ORIENTED_EDGE('',*,*,#3117,.T.);
#4090=ORIENTED_EDGE('',*,*,#3114,.T.);
#4091=ORIENTED_EDGE('',*,*,#3117,.F.);
#4092=ORIENTED_EDGE('',*,*,#3116,.T.);
#4093=ORIENTED_EDGE('',*,*,#3108,.F.);
#4094=ORIENTED_EDGE('',*,*,#3103,.T.);
#4095=ORIENTED_EDGE('',*,*,#3104,.T.);
#4096=ORIENTED_EDGE('',*,*,#3118,.T.);
#4097=ORIENTED_EDGE('',*,*,#3111,.F.);
#4098=ORIENTED_EDGE('',*,*,#3118,.F.);
#4099=ORIENTED_EDGE('',*,*,#3119,.T.);
#4100=ORIENTED_EDGE('',*,*,#3119,.F.);
#4101=ORIENTED_EDGE('',*,*,#3120,.T.);
#4102=ORIENTED_EDGE('',*,*,#3120,.F.);
#4103=ORIENTED_EDGE('',*,*,#3121,.T.);
#4104=ORIENTED_EDGE('',*,*,#3121,.F.);
#4105=ORIENTED_EDGE('',*,*,#3122,.T.);
#4106=ORIENTED_EDGE('',*,*,#3122,.F.);
#4107=ORIENTED_EDGE('',*,*,#3123,.T.);
#4108=ORIENTED_EDGE('',*,*,#3123,.F.);
#4109=ORIENTED_EDGE('',*,*,#3124,.T.);
#4110=ORIENTED_EDGE('',*,*,#3124,.F.);
#4111=ORIENTED_EDGE('',*,*,#3125,.T.);
#4112=ORIENTED_EDGE('',*,*,#3125,.F.);
#4113=ORIENTED_EDGE('',*,*,#3126,.T.);
#4114=ORIENTED_EDGE('',*,*,#3126,.F.);
#4115=ORIENTED_EDGE('',*,*,#3127,.F.);
#4116=ORIENTED_EDGE('',*,*,#3128,.F.);
#4117=ORIENTED_EDGE('',*,*,#3129,.F.);
#4118=ORIENTED_EDGE('',*,*,#3130,.F.);
#4119=ORIENTED_EDGE('',*,*,#3129,.T.);
#4120=ORIENTED_EDGE('',*,*,#3131,.F.);
#4121=ORIENTED_EDGE('',*,*,#3132,.T.);
#4122=ORIENTED_EDGE('',*,*,#3133,.F.);
#4123=ORIENTED_EDGE('',*,*,#3134,.T.);
#4124=ORIENTED_EDGE('',*,*,#3135,.F.);
#4125=ORIENTED_EDGE('',*,*,#3136,.T.);
#4126=ORIENTED_EDGE('',*,*,#3137,.T.);
#4127=ORIENTED_EDGE('',*,*,#3138,.F.);
#4128=ORIENTED_EDGE('',*,*,#3137,.F.);
#4129=ORIENTED_EDGE('',*,*,#3139,.T.);
#4130=ORIENTED_EDGE('',*,*,#3140,.F.);
#4131=ORIENTED_EDGE('',*,*,#3141,.T.);
#4132=ORIENTED_EDGE('',*,*,#3142,.F.);
#4133=ORIENTED_EDGE('',*,*,#3143,.T.);
#4134=ORIENTED_EDGE('',*,*,#3144,.F.);
#4135=ORIENTED_EDGE('',*,*,#3145,.T.);
#4136=ORIENTED_EDGE('',*,*,#3146,.F.);
#4137=ORIENTED_EDGE('',*,*,#3147,.T.);
#4138=ORIENTED_EDGE('',*,*,#3148,.F.);
#4139=ORIENTED_EDGE('',*,*,#3128,.T.);
#4140=ORIENTED_EDGE('',*,*,#3149,.T.);
#4141=ORIENTED_EDGE('',*,*,#3150,.T.);
#4142=ORIENTED_EDGE('',*,*,#3131,.T.);
#4143=ORIENTED_EDGE('',*,*,#3151,.F.);
#4144=ORIENTED_EDGE('',*,*,#3152,.F.);
#4145=ORIENTED_EDGE('',*,*,#3132,.F.);
#4146=ORIENTED_EDGE('',*,*,#3150,.F.);
#4147=ORIENTED_EDGE('',*,*,#3152,.T.);
#4148=ORIENTED_EDGE('',*,*,#3153,.T.);
#4149=ORIENTED_EDGE('',*,*,#3154,.T.);
#4150=ORIENTED_EDGE('',*,*,#3133,.T.);
#4151=ORIENTED_EDGE('',*,*,#3155,.F.);
#4152=ORIENTED_EDGE('',*,*,#3156,.F.);
#4153=ORIENTED_EDGE('',*,*,#3134,.F.);
#4154=ORIENTED_EDGE('',*,*,#3154,.F.);
#4155=ORIENTED_EDGE('',*,*,#3156,.T.);
#4156=ORIENTED_EDGE('',*,*,#3157,.T.);
#4157=ORIENTED_EDGE('',*,*,#3158,.T.);
#4158=ORIENTED_EDGE('',*,*,#3135,.T.);
#4159=ORIENTED_EDGE('',*,*,#3159,.F.);
#4160=ORIENTED_EDGE('',*,*,#3160,.F.);
#4161=ORIENTED_EDGE('',*,*,#3139,.F.);
#4162=ORIENTED_EDGE('',*,*,#3136,.F.);
#4163=ORIENTED_EDGE('',*,*,#3158,.F.);
#4164=ORIENTED_EDGE('',*,*,#3161,.F.);
#4165=ORIENTED_EDGE('',*,*,#3160,.T.);
#4166=ORIENTED_EDGE('',*,*,#3162,.T.);
#4167=ORIENTED_EDGE('',*,*,#3163,.T.);
#4168=ORIENTED_EDGE('',*,*,#3140,.T.);
#4169=ORIENTED_EDGE('',*,*,#3164,.F.);
#4170=ORIENTED_EDGE('',*,*,#3165,.F.);
#4171=ORIENTED_EDGE('',*,*,#3141,.F.);
#4172=ORIENTED_EDGE('',*,*,#3163,.F.);
#4173=ORIENTED_EDGE('',*,*,#3165,.T.);
#4174=ORIENTED_EDGE('',*,*,#3166,.T.);
#4175=ORIENTED_EDGE('',*,*,#3167,.T.);
#4176=ORIENTED_EDGE('',*,*,#3142,.T.);
#4177=ORIENTED_EDGE('',*,*,#3168,.F.);
#4178=ORIENTED_EDGE('',*,*,#3169,.F.);
#4179=ORIENTED_EDGE('',*,*,#3143,.F.);
#4180=ORIENTED_EDGE('',*,*,#3167,.F.);
#4181=ORIENTED_EDGE('',*,*,#3169,.T.);
#4182=ORIENTED_EDGE('',*,*,#3170,.T.);
#4183=ORIENTED_EDGE('',*,*,#3171,.T.);
#4184=ORIENTED_EDGE('',*,*,#3144,.T.);
#4185=ORIENTED_EDGE('',*,*,#3145,.F.);
#4186=ORIENTED_EDGE('',*,*,#3171,.F.);
#4187=ORIENTED_EDGE('',*,*,#3172,.F.);
#4188=ORIENTED_EDGE('',*,*,#3173,.F.);
#4189=ORIENTED_EDGE('',*,*,#3174,.F.);
#4190=ORIENTED_EDGE('',*,*,#3175,.T.);
#4191=ORIENTED_EDGE('',*,*,#3161,.T.);
#4192=ORIENTED_EDGE('',*,*,#3157,.F.);
#4193=ORIENTED_EDGE('',*,*,#3155,.T.);
#4194=ORIENTED_EDGE('',*,*,#3153,.F.);
#4195=ORIENTED_EDGE('',*,*,#3151,.T.);
#4196=ORIENTED_EDGE('',*,*,#3149,.F.);
#4197=ORIENTED_EDGE('',*,*,#3127,.T.);
#4198=ORIENTED_EDGE('',*,*,#3176,.F.);
#4199=ORIENTED_EDGE('',*,*,#3177,.T.);
#4200=ORIENTED_EDGE('',*,*,#3178,.F.);
#4201=ORIENTED_EDGE('',*,*,#3172,.T.);
#4202=ORIENTED_EDGE('',*,*,#3170,.F.);
#4203=ORIENTED_EDGE('',*,*,#3168,.T.);
#4204=ORIENTED_EDGE('',*,*,#3166,.F.);
#4205=ORIENTED_EDGE('',*,*,#3164,.T.);
#4206=ORIENTED_EDGE('',*,*,#3162,.F.);
#4207=ORIENTED_EDGE('',*,*,#3159,.T.);
#4208=ORIENTED_EDGE('',*,*,#3175,.F.);
#4209=ORIENTED_EDGE('',*,*,#3130,.T.);
#4210=ORIENTED_EDGE('',*,*,#3148,.T.);
#4211=ORIENTED_EDGE('',*,*,#3179,.T.);
#4212=ORIENTED_EDGE('',*,*,#3176,.T.);
#4213=ORIENTED_EDGE('',*,*,#3147,.F.);
#4214=ORIENTED_EDGE('',*,*,#3180,.F.);
#4215=ORIENTED_EDGE('',*,*,#3177,.F.);
#4216=ORIENTED_EDGE('',*,*,#3179,.F.);
#4217=ORIENTED_EDGE('',*,*,#3138,.T.);
#4218=ORIENTED_EDGE('',*,*,#3174,.T.);
#4219=ORIENTED_EDGE('',*,*,#3173,.T.);
#4220=ORIENTED_EDGE('',*,*,#3178,.T.);
#4221=ORIENTED_EDGE('',*,*,#3180,.T.);
#4222=ORIENTED_EDGE('',*,*,#3146,.T.);
#4223=ORIENTED_EDGE('',*,*,#3181,.F.);
#4224=ORIENTED_EDGE('',*,*,#3182,.T.);
#4225=ORIENTED_EDGE('',*,*,#3183,.F.);
#4226=ORIENTED_EDGE('',*,*,#3184,.T.);
#4227=ORIENTED_EDGE('',*,*,#3181,.T.);
#4228=ORIENTED_EDGE('',*,*,#3184,.F.);
#4229=ORIENTED_EDGE('',*,*,#3183,.T.);
#4230=ORIENTED_EDGE('',*,*,#3185,.F.);
#4231=ORIENTED_EDGE('',*,*,#3185,.T.);
#4232=ORIENTED_EDGE('',*,*,#3186,.T.);
#4233=ORIENTED_EDGE('',*,*,#3182,.F.);
#4234=ORIENTED_EDGE('',*,*,#3186,.F.);
#4235=ORIENTED_EDGE('',*,*,#3187,.F.);
#4236=ORIENTED_EDGE('',*,*,#3188,.T.);
#4237=ORIENTED_EDGE('',*,*,#3189,.F.);
#4238=ORIENTED_EDGE('',*,*,#3190,.T.);
#4239=ORIENTED_EDGE('',*,*,#3187,.T.);
#4240=ORIENTED_EDGE('',*,*,#3190,.F.);
#4241=ORIENTED_EDGE('',*,*,#3189,.T.);
#4242=ORIENTED_EDGE('',*,*,#3191,.F.);
#4243=ORIENTED_EDGE('',*,*,#3191,.T.);
#4244=ORIENTED_EDGE('',*,*,#3192,.T.);
#4245=ORIENTED_EDGE('',*,*,#3188,.F.);
#4246=ORIENTED_EDGE('',*,*,#3192,.F.);
#4247=ORIENTED_EDGE('',*,*,#3193,.F.);
#4248=ORIENTED_EDGE('',*,*,#3194,.F.);
#4249=ORIENTED_EDGE('',*,*,#3195,.T.);
#4250=ORIENTED_EDGE('',*,*,#3193,.T.);
#4251=ORIENTED_EDGE('',*,*,#3195,.F.);
#4252=ORIENTED_EDGE('',*,*,#3196,.F.);
#4253=ORIENTED_EDGE('',*,*,#3197,.T.);
#4254=ORIENTED_EDGE('',*,*,#3194,.T.);
#4255=ORIENTED_EDGE('',*,*,#3197,.F.);
#4256=ORIENTED_EDGE('',*,*,#3198,.F.);
#4257=ORIENTED_EDGE('',*,*,#3199,.T.);
#4258=ORIENTED_EDGE('',*,*,#3196,.T.);
#4259=ORIENTED_EDGE('',*,*,#3199,.F.);
#4260=ORIENTED_EDGE('',*,*,#3198,.T.);
#4261=ORIENTED_EDGE('',*,*,#3200,.F.);
#4262=ORIENTED_EDGE('',*,*,#3201,.F.);
#4263=ORIENTED_EDGE('',*,*,#3202,.T.);
#4264=ORIENTED_EDGE('',*,*,#3200,.T.);
#4265=ORIENTED_EDGE('',*,*,#3202,.F.);
#4266=ORIENTED_EDGE('',*,*,#3203,.F.);
#4267=ORIENTED_EDGE('',*,*,#3204,.T.);
#4268=ORIENTED_EDGE('',*,*,#3201,.T.);
#4269=ORIENTED_EDGE('',*,*,#3204,.F.);
#4270=ORIENTED_EDGE('',*,*,#3205,.F.);
#4271=ORIENTED_EDGE('',*,*,#3206,.T.);
#4272=ORIENTED_EDGE('',*,*,#3203,.T.);
#4273=ORIENTED_EDGE('',*,*,#3206,.F.);
#4274=ORIENTED_EDGE('',*,*,#3205,.T.);
#4275=ORIENTED_EDGE('',*,*,#3207,.T.);
#4276=ORIENTED_EDGE('',*,*,#3208,.T.);
#4277=ORIENTED_EDGE('',*,*,#3209,.T.);
#4278=ORIENTED_EDGE('',*,*,#3210,.F.);
#4279=ORIENTED_EDGE('',*,*,#3211,.T.);
#4280=ORIENTED_EDGE('',*,*,#3212,.T.);
#4281=ORIENTED_EDGE('',*,*,#3213,.T.);
#4282=ORIENTED_EDGE('',*,*,#3208,.F.);
#4283=ORIENTED_EDGE('',*,*,#3214,.T.);
#4284=ORIENTED_EDGE('',*,*,#3215,.T.);
#4285=ORIENTED_EDGE('',*,*,#3216,.T.);
#4286=ORIENTED_EDGE('',*,*,#3212,.F.);
#4287=ORIENTED_EDGE('',*,*,#3217,.T.);
#4288=ORIENTED_EDGE('',*,*,#3218,.T.);
#4289=ORIENTED_EDGE('',*,*,#3219,.T.);
#4290=ORIENTED_EDGE('',*,*,#3215,.F.);
#4291=ORIENTED_EDGE('',*,*,#3220,.T.);
#4292=ORIENTED_EDGE('',*,*,#3221,.T.);
#4293=ORIENTED_EDGE('',*,*,#3222,.T.);
#4294=ORIENTED_EDGE('',*,*,#3218,.F.);
#4295=ORIENTED_EDGE('',*,*,#3223,.T.);
#4296=ORIENTED_EDGE('',*,*,#3210,.T.);
#4297=ORIENTED_EDGE('',*,*,#3224,.T.);
#4298=ORIENTED_EDGE('',*,*,#3221,.F.);
#4299=ORIENTED_EDGE('',*,*,#3223,.F.);
#4300=ORIENTED_EDGE('',*,*,#3220,.F.);
#4301=ORIENTED_EDGE('',*,*,#3217,.F.);
#4302=ORIENTED_EDGE('',*,*,#3214,.F.);
#4303=ORIENTED_EDGE('',*,*,#3211,.F.);
#4304=ORIENTED_EDGE('',*,*,#3207,.F.);
#4305=ORIENTED_EDGE('',*,*,#3224,.F.);
#4306=ORIENTED_EDGE('',*,*,#3209,.F.);
#4307=ORIENTED_EDGE('',*,*,#3213,.F.);
#4308=ORIENTED_EDGE('',*,*,#3216,.F.);
#4309=ORIENTED_EDGE('',*,*,#3219,.F.);
#4310=ORIENTED_EDGE('',*,*,#3222,.F.);
#4311=ORIENTED_EDGE('',*,*,#3225,.F.);
#4312=ORIENTED_EDGE('',*,*,#3226,.F.);
#4313=ORIENTED_EDGE('',*,*,#3227,.T.);
#4314=ORIENTED_EDGE('',*,*,#3225,.T.);
#4315=ORIENTED_EDGE('',*,*,#3227,.F.);
#4316=ORIENTED_EDGE('',*,*,#3228,.F.);
#4317=ORIENTED_EDGE('',*,*,#3229,.T.);
#4318=ORIENTED_EDGE('',*,*,#3226,.T.);
#4319=ORIENTED_EDGE('',*,*,#3229,.F.);
#4320=ORIENTED_EDGE('',*,*,#3230,.F.);
#4321=ORIENTED_EDGE('',*,*,#3231,.T.);
#4322=ORIENTED_EDGE('',*,*,#3228,.T.);
#4323=ORIENTED_EDGE('',*,*,#3231,.F.);
#4324=ORIENTED_EDGE('',*,*,#3230,.T.);
#4325=ORIENTED_EDGE('',*,*,#3232,.F.);
#4326=ORIENTED_EDGE('',*,*,#3233,.F.);
#4327=ORIENTED_EDGE('',*,*,#3234,.T.);
#4328=ORIENTED_EDGE('',*,*,#3232,.T.);
#4329=ORIENTED_EDGE('',*,*,#3234,.F.);
#4330=ORIENTED_EDGE('',*,*,#3235,.F.);
#4331=ORIENTED_EDGE('',*,*,#3236,.T.);
#4332=ORIENTED_EDGE('',*,*,#3233,.T.);
#4333=ORIENTED_EDGE('',*,*,#3236,.F.);
#4334=ORIENTED_EDGE('',*,*,#3237,.F.);
#4335=ORIENTED_EDGE('',*,*,#3238,.T.);
#4336=ORIENTED_EDGE('',*,*,#3235,.T.);
#4337=ORIENTED_EDGE('',*,*,#3238,.F.);
#4338=ORIENTED_EDGE('',*,*,#3237,.T.);
#4339=ORIENTED_EDGE('',*,*,#3239,.T.);
#4340=ORIENTED_EDGE('',*,*,#3240,.T.);
#4341=ORIENTED_EDGE('',*,*,#3241,.T.);
#4342=ORIENTED_EDGE('',*,*,#3242,.F.);
#4343=ORIENTED_EDGE('',*,*,#3243,.T.);
#4344=ORIENTED_EDGE('',*,*,#3244,.T.);
#4345=ORIENTED_EDGE('',*,*,#3245,.T.);
#4346=ORIENTED_EDGE('',*,*,#3240,.F.);
#4347=ORIENTED_EDGE('',*,*,#3246,.T.);
#4348=ORIENTED_EDGE('',*,*,#3247,.T.);
#4349=ORIENTED_EDGE('',*,*,#3248,.T.);
#4350=ORIENTED_EDGE('',*,*,#3244,.F.);
#4351=ORIENTED_EDGE('',*,*,#3249,.T.);
#4352=ORIENTED_EDGE('',*,*,#3250,.T.);
#4353=ORIENTED_EDGE('',*,*,#3251,.T.);
#4354=ORIENTED_EDGE('',*,*,#3247,.F.);
#4355=ORIENTED_EDGE('',*,*,#3252,.T.);
#4356=ORIENTED_EDGE('',*,*,#3253,.T.);
#4357=ORIENTED_EDGE('',*,*,#3254,.T.);
#4358=ORIENTED_EDGE('',*,*,#3250,.F.);
#4359=ORIENTED_EDGE('',*,*,#3255,.T.);
#4360=ORIENTED_EDGE('',*,*,#3242,.T.);
#4361=ORIENTED_EDGE('',*,*,#3256,.T.);
#4362=ORIENTED_EDGE('',*,*,#3253,.F.);
#4363=ORIENTED_EDGE('',*,*,#3255,.F.);
#4364=ORIENTED_EDGE('',*,*,#3252,.F.);
#4365=ORIENTED_EDGE('',*,*,#3249,.F.);
#4366=ORIENTED_EDGE('',*,*,#3246,.F.);
#4367=ORIENTED_EDGE('',*,*,#3243,.F.);
#4368=ORIENTED_EDGE('',*,*,#3239,.F.);
#4369=ORIENTED_EDGE('',*,*,#3256,.F.);
#4370=ORIENTED_EDGE('',*,*,#3241,.F.);
#4371=ORIENTED_EDGE('',*,*,#3245,.F.);
#4372=ORIENTED_EDGE('',*,*,#3248,.F.);
#4373=ORIENTED_EDGE('',*,*,#3251,.F.);
#4374=ORIENTED_EDGE('',*,*,#3254,.F.);
#4375=ORIENTED_EDGE('',*,*,#3257,.F.);
#4376=ORIENTED_EDGE('',*,*,#3258,.T.);
#4377=ORIENTED_EDGE('',*,*,#3259,.F.);
#4378=ORIENTED_EDGE('',*,*,#3260,.T.);
#4379=ORIENTED_EDGE('',*,*,#3261,.F.);
#4380=ORIENTED_EDGE('',*,*,#3260,.F.);
#4381=ORIENTED_EDGE('',*,*,#3262,.F.);
#4382=ORIENTED_EDGE('',*,*,#3263,.F.);
#4383=ORIENTED_EDGE('',*,*,#3264,.F.);
#4384=ORIENTED_EDGE('',*,*,#3263,.T.);
#4385=ORIENTED_EDGE('',*,*,#3265,.T.);
#4386=ORIENTED_EDGE('',*,*,#3266,.T.);
#4387=ORIENTED_EDGE('',*,*,#3262,.T.);
#4388=ORIENTED_EDGE('',*,*,#3259,.T.);
#4389=ORIENTED_EDGE('',*,*,#3267,.T.);
#4390=ORIENTED_EDGE('',*,*,#3265,.F.);
#4391=ORIENTED_EDGE('',*,*,#3268,.F.);
#4392=ORIENTED_EDGE('',*,*,#3266,.F.);
#4393=ORIENTED_EDGE('',*,*,#3267,.F.);
#4394=ORIENTED_EDGE('',*,*,#3258,.F.);
#4395=ORIENTED_EDGE('',*,*,#3269,.F.);
#4396=ORIENTED_EDGE('',*,*,#3270,.T.);
#4397=ORIENTED_EDGE('',*,*,#3271,.F.);
#4398=ORIENTED_EDGE('',*,*,#3270,.F.);
#4399=ORIENTED_EDGE('',*,*,#3264,.T.);
#4400=ORIENTED_EDGE('',*,*,#3268,.T.);
#4401=ORIENTED_EDGE('',*,*,#3257,.T.);
#4402=ORIENTED_EDGE('',*,*,#3261,.T.);
#4403=ORIENTED_EDGE('',*,*,#3269,.T.);
#4404=ORIENTED_EDGE('',*,*,#3272,.T.);
#4405=ORIENTED_EDGE('',*,*,#3273,.F.);
#4406=ORIENTED_EDGE('',*,*,#3274,.F.);
#4407=ORIENTED_EDGE('',*,*,#3275,.F.);
#4408=ORIENTED_EDGE('',*,*,#3272,.F.);
#4409=ORIENTED_EDGE('',*,*,#3276,.T.);
#4410=ORIENTED_EDGE('',*,*,#3274,.T.);
#4411=ORIENTED_EDGE('',*,*,#3276,.F.);
#4412=ORIENTED_EDGE('',*,*,#3275,.T.);
#4413=ORIENTED_EDGE('',*,*,#3277,.T.);
#4414=ORIENTED_EDGE('',*,*,#3278,.T.);
#4415=ORIENTED_EDGE('',*,*,#3277,.F.);
#4416=ORIENTED_EDGE('',*,*,#3279,.F.);
#4417=ORIENTED_EDGE('',*,*,#3280,.T.);
#4418=ORIENTED_EDGE('',*,*,#3273,.T.);
#4419=ORIENTED_EDGE('',*,*,#3280,.F.);
#4420=ORIENTED_EDGE('',*,*,#3279,.T.);
#4421=ORIENTED_EDGE('',*,*,#3271,.T.);
#4422=ORIENTED_EDGE('',*,*,#3278,.F.);
#4423=ORIENTED_EDGE('',*,*,#3281,.F.);
#4424=ORIENTED_EDGE('',*,*,#3282,.T.);
#4425=ORIENTED_EDGE('',*,*,#3283,.T.);
#4426=ORIENTED_EDGE('',*,*,#3282,.F.);
#4427=ORIENTED_EDGE('',*,*,#3284,.F.);
#4428=ORIENTED_EDGE('',*,*,#3285,.T.);
#4429=ORIENTED_EDGE('',*,*,#3286,.T.);
#4430=ORIENTED_EDGE('',*,*,#3285,.F.);
#4431=ORIENTED_EDGE('',*,*,#3284,.T.);
#4432=ORIENTED_EDGE('',*,*,#3281,.T.);
#4433=ORIENTED_EDGE('',*,*,#3286,.F.);
#4434=ORIENTED_EDGE('',*,*,#3283,.F.);
#4435=ORIENTED_EDGE('',*,*,#3287,.F.);
#4436=ORIENTED_EDGE('',*,*,#3288,.T.);
#4437=ORIENTED_EDGE('',*,*,#3289,.F.);
#4438=ORIENTED_EDGE('',*,*,#3290,.F.);
#4439=ORIENTED_EDGE('',*,*,#3291,.T.);
#4440=ORIENTED_EDGE('',*,*,#3292,.F.);
#4441=ORIENTED_EDGE('',*,*,#3293,.F.);
#4442=ORIENTED_EDGE('',*,*,#3291,.F.);
#4443=ORIENTED_EDGE('',*,*,#3294,.F.);
#4444=ORIENTED_EDGE('',*,*,#3295,.F.);
#4445=ORIENTED_EDGE('',*,*,#3288,.F.);
#4446=ORIENTED_EDGE('',*,*,#3296,.F.);
#4447=ORIENTED_EDGE('',*,*,#3294,.T.);
#4448=ORIENTED_EDGE('',*,*,#3290,.T.);
#4449=ORIENTED_EDGE('',*,*,#3297,.F.);
#4450=ORIENTED_EDGE('',*,*,#3298,.T.);
#4451=ORIENTED_EDGE('',*,*,#3299,.T.);
#4452=ORIENTED_EDGE('',*,*,#3298,.F.);
#4453=ORIENTED_EDGE('',*,*,#3295,.T.);
#4454=ORIENTED_EDGE('',*,*,#3296,.T.);
#4455=ORIENTED_EDGE('',*,*,#3289,.T.);
#4456=ORIENTED_EDGE('',*,*,#3287,.T.);
#4457=ORIENTED_EDGE('',*,*,#3300,.F.);
#4458=ORIENTED_EDGE('',*,*,#3301,.T.);
#4459=ORIENTED_EDGE('',*,*,#3302,.T.);
#4460=ORIENTED_EDGE('',*,*,#3301,.F.);
#4461=ORIENTED_EDGE('',*,*,#3292,.T.);
#4462=ORIENTED_EDGE('',*,*,#3293,.T.);
#4463=ORIENTED_EDGE('',*,*,#3300,.T.);
#4464=ORIENTED_EDGE('',*,*,#3297,.T.);
#4465=ORIENTED_EDGE('',*,*,#3302,.F.);
#4466=ORIENTED_EDGE('',*,*,#3299,.F.);
#4467=ORIENTED_EDGE('',*,*,#3303,.F.);
#4468=ORIENTED_EDGE('',*,*,#3304,.T.);
#4469=ORIENTED_EDGE('',*,*,#3305,.F.);
#4470=ORIENTED_EDGE('',*,*,#3306,.F.);
#4471=ORIENTED_EDGE('',*,*,#3307,.T.);
#4472=ORIENTED_EDGE('',*,*,#3308,.F.);
#4473=ORIENTED_EDGE('',*,*,#3309,.F.);
#4474=ORIENTED_EDGE('',*,*,#3307,.F.);
#4475=ORIENTED_EDGE('',*,*,#3310,.F.);
#4476=ORIENTED_EDGE('',*,*,#3311,.F.);
#4477=ORIENTED_EDGE('',*,*,#3304,.F.);
#4478=ORIENTED_EDGE('',*,*,#3312,.F.);
#4479=ORIENTED_EDGE('',*,*,#3310,.T.);
#4480=ORIENTED_EDGE('',*,*,#3306,.T.);
#4481=ORIENTED_EDGE('',*,*,#3313,.F.);
#4482=ORIENTED_EDGE('',*,*,#3314,.T.);
#4483=ORIENTED_EDGE('',*,*,#3315,.T.);
#4484=ORIENTED_EDGE('',*,*,#3314,.F.);
#4485=ORIENTED_EDGE('',*,*,#3311,.T.);
#4486=ORIENTED_EDGE('',*,*,#3312,.T.);
#4487=ORIENTED_EDGE('',*,*,#3305,.T.);
#4488=ORIENTED_EDGE('',*,*,#3303,.T.);
#4489=ORIENTED_EDGE('',*,*,#3316,.F.);
#4490=ORIENTED_EDGE('',*,*,#3317,.T.);
#4491=ORIENTED_EDGE('',*,*,#3318,.T.);
#4492=ORIENTED_EDGE('',*,*,#3317,.F.);
#4493=ORIENTED_EDGE('',*,*,#3308,.T.);
#4494=ORIENTED_EDGE('',*,*,#3309,.T.);
#4495=ORIENTED_EDGE('',*,*,#3316,.T.);
#4496=ORIENTED_EDGE('',*,*,#3313,.T.);
#4497=ORIENTED_EDGE('',*,*,#3318,.F.);
#4498=ORIENTED_EDGE('',*,*,#3315,.F.);
#4499=ORIENTED_EDGE('',*,*,#3319,.F.);
#4500=ORIENTED_EDGE('',*,*,#3320,.T.);
#4501=ORIENTED_EDGE('',*,*,#3321,.F.);
#4502=ORIENTED_EDGE('',*,*,#3322,.F.);
#4503=ORIENTED_EDGE('',*,*,#3323,.F.);
#4504=ORIENTED_EDGE('',*,*,#3324,.T.);
#4505=ORIENTED_EDGE('',*,*,#3325,.F.);
#4506=ORIENTED_EDGE('',*,*,#3320,.F.);
#4507=ORIENTED_EDGE('',*,*,#3326,.F.);
#4508=ORIENTED_EDGE('',*,*,#3327,.F.);
#4509=ORIENTED_EDGE('',*,*,#3328,.F.);
#4510=ORIENTED_EDGE('',*,*,#3329,.F.);
#4511=ORIENTED_EDGE('',*,*,#3324,.F.);
#4512=ORIENTED_EDGE('',*,*,#3330,.T.);
#4513=ORIENTED_EDGE('',*,*,#3321,.T.);
#4514=ORIENTED_EDGE('',*,*,#3325,.T.);
#4515=ORIENTED_EDGE('',*,*,#3329,.T.);
#4516=ORIENTED_EDGE('',*,*,#3331,.T.);
#4517=ORIENTED_EDGE('',*,*,#3322,.T.);
#4518=ORIENTED_EDGE('',*,*,#3331,.F.);
#4519=ORIENTED_EDGE('',*,*,#3328,.T.);
#4520=ORIENTED_EDGE('',*,*,#3332,.F.);
#4521=ORIENTED_EDGE('',*,*,#3333,.T.);
#4522=ORIENTED_EDGE('',*,*,#3334,.T.);
#4523=ORIENTED_EDGE('',*,*,#3335,.T.);
#4524=ORIENTED_EDGE('',*,*,#3336,.T.);
#4525=ORIENTED_EDGE('',*,*,#3337,.T.);
#4526=ORIENTED_EDGE('',*,*,#3338,.T.);
#4527=ORIENTED_EDGE('',*,*,#3339,.F.);
#4528=ORIENTED_EDGE('',*,*,#3340,.F.);
#4529=ORIENTED_EDGE('',*,*,#3341,.F.);
#4530=ORIENTED_EDGE('',*,*,#3342,.T.);
#4531=ORIENTED_EDGE('',*,*,#3335,.F.);
#4532=ORIENTED_EDGE('',*,*,#3336,.F.);
#4533=ORIENTED_EDGE('',*,*,#3342,.F.);
#4534=ORIENTED_EDGE('',*,*,#3337,.F.);
#4535=ORIENTED_EDGE('',*,*,#3338,.F.);
#4536=ORIENTED_EDGE('',*,*,#3343,.T.);
#4537=ORIENTED_EDGE('',*,*,#3344,.F.);
#4538=ORIENTED_EDGE('',*,*,#3345,.F.);
#4539=ORIENTED_EDGE('',*,*,#3346,.F.);
#4540=ORIENTED_EDGE('',*,*,#3343,.F.);
#4541=ORIENTED_EDGE('',*,*,#3347,.F.);
#4542=ORIENTED_EDGE('',*,*,#3348,.T.);
#4543=ORIENTED_EDGE('',*,*,#3340,.T.);
#4544=ORIENTED_EDGE('',*,*,#3349,.T.);
#4545=ORIENTED_EDGE('',*,*,#3350,.F.);
#4546=ORIENTED_EDGE('',*,*,#3349,.F.);
#4547=ORIENTED_EDGE('',*,*,#3339,.T.);
#4548=ORIENTED_EDGE('',*,*,#3341,.T.);
#4549=ORIENTED_EDGE('',*,*,#3348,.F.);
#4550=ORIENTED_EDGE('',*,*,#3345,.T.);
#4551=ORIENTED_EDGE('',*,*,#3344,.T.);
#4552=ORIENTED_EDGE('',*,*,#3346,.T.);
#4553=ORIENTED_EDGE('',*,*,#3351,.T.);
#4554=ORIENTED_EDGE('',*,*,#3352,.T.);
#4555=ORIENTED_EDGE('',*,*,#3353,.T.);
#4556=ORIENTED_EDGE('',*,*,#3354,.T.);
#4557=ORIENTED_EDGE('',*,*,#3355,.T.);
#4558=ORIENTED_EDGE('',*,*,#3356,.T.);
#4559=ORIENTED_EDGE('',*,*,#3352,.F.);
#4560=ORIENTED_EDGE('',*,*,#3351,.F.);
#4561=ORIENTED_EDGE('',*,*,#3353,.F.);
#4562=ORIENTED_EDGE('',*,*,#3357,.T.);
#4563=ORIENTED_EDGE('',*,*,#3326,.T.);
#4564=ORIENTED_EDGE('',*,*,#3357,.F.);
#4565=ORIENTED_EDGE('',*,*,#3333,.F.);
#4566=ORIENTED_EDGE('',*,*,#3334,.F.);
#4567=ORIENTED_EDGE('',*,*,#3358,.T.);
#4568=ORIENTED_EDGE('',*,*,#3355,.F.);
#4569=ORIENTED_EDGE('',*,*,#3354,.F.);
#4570=ORIENTED_EDGE('',*,*,#3356,.F.);
#4571=ORIENTED_EDGE('',*,*,#3358,.F.);
#4572=ORIENTED_EDGE('',*,*,#3347,.T.);
#4573=ORIENTED_EDGE('',*,*,#3319,.T.);
#4574=ORIENTED_EDGE('',*,*,#3332,.T.);
#4575=ORIENTED_EDGE('',*,*,#3327,.T.);
#4576=ORIENTED_EDGE('',*,*,#3323,.T.);
#4577=ORIENTED_EDGE('',*,*,#3359,.T.);
#4578=ORIENTED_EDGE('',*,*,#3360,.T.);
#4579=ORIENTED_EDGE('',*,*,#3361,.F.);
#4580=ORIENTED_EDGE('',*,*,#3362,.T.);
#4581=ORIENTED_EDGE('',*,*,#3363,.F.);
#4582=ORIENTED_EDGE('',*,*,#3364,.T.);
#4583=ORIENTED_EDGE('',*,*,#3365,.F.);
#4584=ORIENTED_EDGE('',*,*,#3366,.T.);
#4585=ORIENTED_EDGE('',*,*,#3367,.F.);
#4586=ORIENTED_EDGE('',*,*,#3368,.T.);
#4587=ORIENTED_EDGE('',*,*,#3369,.F.);
#4588=ORIENTED_EDGE('',*,*,#3370,.T.);
#4589=ORIENTED_EDGE('',*,*,#3371,.F.);
#4590=ORIENTED_EDGE('',*,*,#3372,.T.);
#4591=ORIENTED_EDGE('',*,*,#3373,.F.);
#4592=ORIENTED_EDGE('',*,*,#3374,.T.);
#4593=ORIENTED_EDGE('',*,*,#3375,.F.);
#4594=ORIENTED_EDGE('',*,*,#3376,.T.);
#4595=ORIENTED_EDGE('',*,*,#3377,.F.);
#4596=ORIENTED_EDGE('',*,*,#3378,.T.);
#4597=ORIENTED_EDGE('',*,*,#3379,.F.);
#4598=ORIENTED_EDGE('',*,*,#3380,.T.);
#4599=ORIENTED_EDGE('',*,*,#3381,.F.);
#4600=ORIENTED_EDGE('',*,*,#3382,.T.);
#4601=ORIENTED_EDGE('',*,*,#3383,.F.);
#4602=ORIENTED_EDGE('',*,*,#3384,.T.);
#4603=ORIENTED_EDGE('',*,*,#3385,.F.);
#4604=ORIENTED_EDGE('',*,*,#3386,.T.);
#4605=ORIENTED_EDGE('',*,*,#3387,.F.);
#4606=ORIENTED_EDGE('',*,*,#3388,.T.);
#4607=ORIENTED_EDGE('',*,*,#3389,.F.);
#4608=ORIENTED_EDGE('',*,*,#3390,.T.);
#4609=ORIENTED_EDGE('',*,*,#3391,.F.);
#4610=ORIENTED_EDGE('',*,*,#3392,.T.);
#4611=ORIENTED_EDGE('',*,*,#3393,.F.);
#4612=ORIENTED_EDGE('',*,*,#3394,.T.);
#4613=ORIENTED_EDGE('',*,*,#3395,.F.);
#4614=ORIENTED_EDGE('',*,*,#3396,.T.);
#4615=ORIENTED_EDGE('',*,*,#3397,.F.);
#4616=ORIENTED_EDGE('',*,*,#3398,.T.);
#4617=ORIENTED_EDGE('',*,*,#3399,.F.);
#4618=ORIENTED_EDGE('',*,*,#3400,.T.);
#4619=ORIENTED_EDGE('',*,*,#3401,.F.);
#4620=ORIENTED_EDGE('',*,*,#3402,.T.);
#4621=ORIENTED_EDGE('',*,*,#3403,.F.);
#4622=ORIENTED_EDGE('',*,*,#3404,.T.);
#4623=ORIENTED_EDGE('',*,*,#3405,.F.);
#4624=ORIENTED_EDGE('',*,*,#3406,.T.);
#4625=ORIENTED_EDGE('',*,*,#3407,.F.);
#4626=ORIENTED_EDGE('',*,*,#3408,.T.);
#4627=ORIENTED_EDGE('',*,*,#3409,.F.);
#4628=ORIENTED_EDGE('',*,*,#3410,.T.);
#4629=ORIENTED_EDGE('',*,*,#3411,.F.);
#4630=ORIENTED_EDGE('',*,*,#3412,.T.);
#4631=ORIENTED_EDGE('',*,*,#3413,.F.);
#4632=ORIENTED_EDGE('',*,*,#3414,.T.);
#4633=ORIENTED_EDGE('',*,*,#3415,.F.);
#4634=ORIENTED_EDGE('',*,*,#3416,.T.);
#4635=ORIENTED_EDGE('',*,*,#3417,.F.);
#4636=ORIENTED_EDGE('',*,*,#3418,.T.);
#4637=ORIENTED_EDGE('',*,*,#3419,.F.);
#4638=ORIENTED_EDGE('',*,*,#3420,.T.);
#4639=ORIENTED_EDGE('',*,*,#3421,.F.);
#4640=ORIENTED_EDGE('',*,*,#3422,.T.);
#4641=ORIENTED_EDGE('',*,*,#3423,.F.);
#4642=ORIENTED_EDGE('',*,*,#3424,.T.);
#4643=ORIENTED_EDGE('',*,*,#3425,.F.);
#4644=ORIENTED_EDGE('',*,*,#3426,.T.);
#4645=ORIENTED_EDGE('',*,*,#3427,.F.);
#4646=ORIENTED_EDGE('',*,*,#3428,.T.);
#4647=ORIENTED_EDGE('',*,*,#3429,.F.);
#4648=ORIENTED_EDGE('',*,*,#3430,.T.);
#4649=ORIENTED_EDGE('',*,*,#3431,.F.);
#4650=ORIENTED_EDGE('',*,*,#3432,.T.);
#4651=ORIENTED_EDGE('',*,*,#3433,.F.);
#4652=ORIENTED_EDGE('',*,*,#3434,.T.);
#4653=ORIENTED_EDGE('',*,*,#3435,.F.);
#4654=ORIENTED_EDGE('',*,*,#3436,.T.);
#4655=ORIENTED_EDGE('',*,*,#3437,.F.);
#4656=ORIENTED_EDGE('',*,*,#3438,.T.);
#4657=ORIENTED_EDGE('',*,*,#3439,.F.);
#4658=ORIENTED_EDGE('',*,*,#3440,.F.);
#4659=ORIENTED_EDGE('',*,*,#3441,.T.);
#4660=ORIENTED_EDGE('',*,*,#3359,.F.);
#4661=ORIENTED_EDGE('',*,*,#3441,.F.);
#4662=ORIENTED_EDGE('',*,*,#3440,.T.);
#4663=ORIENTED_EDGE('',*,*,#3350,.T.);
#4664=ORIENTED_EDGE('',*,*,#3442,.F.);
#4665=ORIENTED_EDGE('',*,*,#3443,.T.);
#4666=ORIENTED_EDGE('',*,*,#3444,.T.);
#4667=ORIENTED_EDGE('',*,*,#3445,.T.);
#4668=ORIENTED_EDGE('',*,*,#3446,.T.);
#4669=ORIENTED_EDGE('',*,*,#3447,.T.);
#4670=ORIENTED_EDGE('',*,*,#3448,.T.);
#4671=ORIENTED_EDGE('',*,*,#3449,.T.);
#4672=ORIENTED_EDGE('',*,*,#3450,.T.);
#4673=ORIENTED_EDGE('',*,*,#3451,.T.);
#4674=ORIENTED_EDGE('',*,*,#3452,.T.);
#4675=ORIENTED_EDGE('',*,*,#3453,.T.);
#4676=ORIENTED_EDGE('',*,*,#3454,.T.);
#4677=ORIENTED_EDGE('',*,*,#3455,.T.);
#4678=ORIENTED_EDGE('',*,*,#3456,.T.);
#4679=ORIENTED_EDGE('',*,*,#3457,.T.);
#4680=ORIENTED_EDGE('',*,*,#3458,.T.);
#4681=ORIENTED_EDGE('',*,*,#3459,.T.);
#4682=ORIENTED_EDGE('',*,*,#3460,.T.);
#4683=ORIENTED_EDGE('',*,*,#3461,.T.);
#4684=ORIENTED_EDGE('',*,*,#3462,.T.);
#4685=ORIENTED_EDGE('',*,*,#3463,.T.);
#4686=ORIENTED_EDGE('',*,*,#3464,.T.);
#4687=ORIENTED_EDGE('',*,*,#3465,.T.);
#4688=ORIENTED_EDGE('',*,*,#3466,.T.);
#4689=ORIENTED_EDGE('',*,*,#3467,.T.);
#4690=ORIENTED_EDGE('',*,*,#3468,.T.);
#4691=ORIENTED_EDGE('',*,*,#3469,.T.);
#4692=ORIENTED_EDGE('',*,*,#3470,.T.);
#4693=ORIENTED_EDGE('',*,*,#3471,.T.);
#4694=ORIENTED_EDGE('',*,*,#3472,.T.);
#4695=ORIENTED_EDGE('',*,*,#3473,.T.);
#4696=ORIENTED_EDGE('',*,*,#3474,.T.);
#4697=ORIENTED_EDGE('',*,*,#3475,.T.);
#4698=ORIENTED_EDGE('',*,*,#3476,.T.);
#4699=ORIENTED_EDGE('',*,*,#3477,.T.);
#4700=ORIENTED_EDGE('',*,*,#3478,.T.);
#4701=ORIENTED_EDGE('',*,*,#3479,.T.);
#4702=ORIENTED_EDGE('',*,*,#3480,.T.);
#4703=ORIENTED_EDGE('',*,*,#3481,.T.);
#4704=ORIENTED_EDGE('',*,*,#3482,.T.);
#4705=ORIENTED_EDGE('',*,*,#3483,.T.);
#4706=ORIENTED_EDGE('',*,*,#3484,.T.);
#4707=ORIENTED_EDGE('',*,*,#3485,.T.);
#4708=ORIENTED_EDGE('',*,*,#3486,.T.);
#4709=ORIENTED_EDGE('',*,*,#3487,.T.);
#4710=ORIENTED_EDGE('',*,*,#3488,.T.);
#4711=ORIENTED_EDGE('',*,*,#3489,.T.);
#4712=ORIENTED_EDGE('',*,*,#3490,.T.);
#4713=ORIENTED_EDGE('',*,*,#3491,.T.);
#4714=ORIENTED_EDGE('',*,*,#3492,.T.);
#4715=ORIENTED_EDGE('',*,*,#3493,.T.);
#4716=ORIENTED_EDGE('',*,*,#3494,.T.);
#4717=ORIENTED_EDGE('',*,*,#3495,.T.);
#4718=ORIENTED_EDGE('',*,*,#3496,.T.);
#4719=ORIENTED_EDGE('',*,*,#3497,.T.);
#4720=ORIENTED_EDGE('',*,*,#3498,.T.);
#4721=ORIENTED_EDGE('',*,*,#3499,.T.);
#4722=ORIENTED_EDGE('',*,*,#3500,.T.);
#4723=ORIENTED_EDGE('',*,*,#3501,.T.);
#4724=ORIENTED_EDGE('',*,*,#3502,.T.);
#4725=ORIENTED_EDGE('',*,*,#3503,.T.);
#4726=ORIENTED_EDGE('',*,*,#3504,.T.);
#4727=ORIENTED_EDGE('',*,*,#3505,.T.);
#4728=ORIENTED_EDGE('',*,*,#3506,.T.);
#4729=ORIENTED_EDGE('',*,*,#3507,.T.);
#4730=ORIENTED_EDGE('',*,*,#3508,.T.);
#4731=ORIENTED_EDGE('',*,*,#3509,.T.);
#4732=ORIENTED_EDGE('',*,*,#3510,.T.);
#4733=ORIENTED_EDGE('',*,*,#3511,.T.);
#4734=ORIENTED_EDGE('',*,*,#3512,.T.);
#4735=ORIENTED_EDGE('',*,*,#3513,.T.);
#4736=ORIENTED_EDGE('',*,*,#3514,.T.);
#4737=ORIENTED_EDGE('',*,*,#3515,.T.);
#4738=ORIENTED_EDGE('',*,*,#3516,.T.);
#4739=ORIENTED_EDGE('',*,*,#3517,.T.);
#4740=ORIENTED_EDGE('',*,*,#3518,.T.);
#4741=ORIENTED_EDGE('',*,*,#3519,.T.);
#4742=ORIENTED_EDGE('',*,*,#3520,.T.);
#4743=ORIENTED_EDGE('',*,*,#3521,.T.);
#4744=ORIENTED_EDGE('',*,*,#3522,.T.);
#4745=ORIENTED_EDGE('',*,*,#3330,.F.);
#4746=ORIENTED_EDGE('',*,*,#3523,.T.);
#4747=ORIENTED_EDGE('',*,*,#3442,.T.);
#4748=ORIENTED_EDGE('',*,*,#3523,.F.);
#4749=ORIENTED_EDGE('',*,*,#3524,.F.);
#4750=ORIENTED_EDGE('',*,*,#3443,.F.);
#4751=ORIENTED_EDGE('',*,*,#3525,.F.);
#4752=ORIENTED_EDGE('',*,*,#3360,.F.);
#4753=ORIENTED_EDGE('',*,*,#3525,.T.);
#4754=ORIENTED_EDGE('',*,*,#3522,.F.);
#4755=ORIENTED_EDGE('',*,*,#3526,.T.);
#4756=ORIENTED_EDGE('',*,*,#3361,.T.);
#4757=ORIENTED_EDGE('',*,*,#3526,.F.);
#4758=ORIENTED_EDGE('',*,*,#3521,.F.);
#4759=ORIENTED_EDGE('',*,*,#3527,.F.);
#4760=ORIENTED_EDGE('',*,*,#3362,.F.);
#4761=ORIENTED_EDGE('',*,*,#3527,.T.);
#4762=ORIENTED_EDGE('',*,*,#3520,.F.);
#4763=ORIENTED_EDGE('',*,*,#3528,.T.);
#4764=ORIENTED_EDGE('',*,*,#3363,.T.);
#4765=ORIENTED_EDGE('',*,*,#3528,.F.);
#4766=ORIENTED_EDGE('',*,*,#3519,.F.);
#4767=ORIENTED_EDGE('',*,*,#3529,.F.);
#4768=ORIENTED_EDGE('',*,*,#3364,.F.);
#4769=ORIENTED_EDGE('',*,*,#3529,.T.);
#4770=ORIENTED_EDGE('',*,*,#3518,.F.);
#4771=ORIENTED_EDGE('',*,*,#3530,.T.);
#4772=ORIENTED_EDGE('',*,*,#3365,.T.);
#4773=ORIENTED_EDGE('',*,*,#3530,.F.);
#4774=ORIENTED_EDGE('',*,*,#3517,.F.);
#4775=ORIENTED_EDGE('',*,*,#3531,.F.);
#4776=ORIENTED_EDGE('',*,*,#3366,.F.);
#4777=ORIENTED_EDGE('',*,*,#3531,.T.);
#4778=ORIENTED_EDGE('',*,*,#3516,.F.);
#4779=ORIENTED_EDGE('',*,*,#3532,.T.);
#4780=ORIENTED_EDGE('',*,*,#3367,.T.);
#4781=ORIENTED_EDGE('',*,*,#3532,.F.);
#4782=ORIENTED_EDGE('',*,*,#3515,.F.);
#4783=ORIENTED_EDGE('',*,*,#3533,.F.);
#4784=ORIENTED_EDGE('',*,*,#3368,.F.);
#4785=ORIENTED_EDGE('',*,*,#3533,.T.);
#4786=ORIENTED_EDGE('',*,*,#3514,.F.);
#4787=ORIENTED_EDGE('',*,*,#3534,.T.);
#4788=ORIENTED_EDGE('',*,*,#3369,.T.);
#4789=ORIENTED_EDGE('',*,*,#3534,.F.);
#4790=ORIENTED_EDGE('',*,*,#3513,.F.);
#4791=ORIENTED_EDGE('',*,*,#3535,.F.);
#4792=ORIENTED_EDGE('',*,*,#3370,.F.);
#4793=ORIENTED_EDGE('',*,*,#3535,.T.);
#4794=ORIENTED_EDGE('',*,*,#3512,.F.);
#4795=ORIENTED_EDGE('',*,*,#3536,.T.);
#4796=ORIENTED_EDGE('',*,*,#3371,.T.);
#4797=ORIENTED_EDGE('',*,*,#3536,.F.);
#4798=ORIENTED_EDGE('',*,*,#3511,.F.);
#4799=ORIENTED_EDGE('',*,*,#3537,.F.);
#4800=ORIENTED_EDGE('',*,*,#3372,.F.);
#4801=ORIENTED_EDGE('',*,*,#3537,.T.);
#4802=ORIENTED_EDGE('',*,*,#3510,.F.);
#4803=ORIENTED_EDGE('',*,*,#3538,.T.);
#4804=ORIENTED_EDGE('',*,*,#3373,.T.);
#4805=ORIENTED_EDGE('',*,*,#3538,.F.);
#4806=ORIENTED_EDGE('',*,*,#3509,.F.);
#4807=ORIENTED_EDGE('',*,*,#3539,.F.);
#4808=ORIENTED_EDGE('',*,*,#3374,.F.);
#4809=ORIENTED_EDGE('',*,*,#3539,.T.);
#4810=ORIENTED_EDGE('',*,*,#3508,.F.);
#4811=ORIENTED_EDGE('',*,*,#3540,.T.);
#4812=ORIENTED_EDGE('',*,*,#3375,.T.);
#4813=ORIENTED_EDGE('',*,*,#3540,.F.);
#4814=ORIENTED_EDGE('',*,*,#3507,.F.);
#4815=ORIENTED_EDGE('',*,*,#3541,.F.);
#4816=ORIENTED_EDGE('',*,*,#3376,.F.);
#4817=ORIENTED_EDGE('',*,*,#3541,.T.);
#4818=ORIENTED_EDGE('',*,*,#3506,.F.);
#4819=ORIENTED_EDGE('',*,*,#3542,.T.);
#4820=ORIENTED_EDGE('',*,*,#3377,.T.);
#4821=ORIENTED_EDGE('',*,*,#3542,.F.);
#4822=ORIENTED_EDGE('',*,*,#3505,.F.);
#4823=ORIENTED_EDGE('',*,*,#3543,.F.);
#4824=ORIENTED_EDGE('',*,*,#3378,.F.);
#4825=ORIENTED_EDGE('',*,*,#3543,.T.);
#4826=ORIENTED_EDGE('',*,*,#3504,.F.);
#4827=ORIENTED_EDGE('',*,*,#3544,.T.);
#4828=ORIENTED_EDGE('',*,*,#3379,.T.);
#4829=ORIENTED_EDGE('',*,*,#3544,.F.);
#4830=ORIENTED_EDGE('',*,*,#3503,.F.);
#4831=ORIENTED_EDGE('',*,*,#3545,.F.);
#4832=ORIENTED_EDGE('',*,*,#3380,.F.);
#4833=ORIENTED_EDGE('',*,*,#3545,.T.);
#4834=ORIENTED_EDGE('',*,*,#3502,.F.);
#4835=ORIENTED_EDGE('',*,*,#3546,.T.);
#4836=ORIENTED_EDGE('',*,*,#3381,.T.);
#4837=ORIENTED_EDGE('',*,*,#3546,.F.);
#4838=ORIENTED_EDGE('',*,*,#3501,.F.);
#4839=ORIENTED_EDGE('',*,*,#3547,.F.);
#4840=ORIENTED_EDGE('',*,*,#3382,.F.);
#4841=ORIENTED_EDGE('',*,*,#3547,.T.);
#4842=ORIENTED_EDGE('',*,*,#3500,.F.);
#4843=ORIENTED_EDGE('',*,*,#3548,.T.);
#4844=ORIENTED_EDGE('',*,*,#3383,.T.);
#4845=ORIENTED_EDGE('',*,*,#3548,.F.);
#4846=ORIENTED_EDGE('',*,*,#3499,.F.);
#4847=ORIENTED_EDGE('',*,*,#3549,.F.);
#4848=ORIENTED_EDGE('',*,*,#3384,.F.);
#4849=ORIENTED_EDGE('',*,*,#3549,.T.);
#4850=ORIENTED_EDGE('',*,*,#3498,.F.);
#4851=ORIENTED_EDGE('',*,*,#3550,.T.);
#4852=ORIENTED_EDGE('',*,*,#3385,.T.);
#4853=ORIENTED_EDGE('',*,*,#3550,.F.);
#4854=ORIENTED_EDGE('',*,*,#3497,.F.);
#4855=ORIENTED_EDGE('',*,*,#3551,.F.);
#4856=ORIENTED_EDGE('',*,*,#3386,.F.);
#4857=ORIENTED_EDGE('',*,*,#3551,.T.);
#4858=ORIENTED_EDGE('',*,*,#3496,.F.);
#4859=ORIENTED_EDGE('',*,*,#3552,.T.);
#4860=ORIENTED_EDGE('',*,*,#3387,.T.);
#4861=ORIENTED_EDGE('',*,*,#3552,.F.);
#4862=ORIENTED_EDGE('',*,*,#3495,.F.);
#4863=ORIENTED_EDGE('',*,*,#3553,.F.);
#4864=ORIENTED_EDGE('',*,*,#3388,.F.);
#4865=ORIENTED_EDGE('',*,*,#3553,.T.);
#4866=ORIENTED_EDGE('',*,*,#3494,.F.);
#4867=ORIENTED_EDGE('',*,*,#3554,.T.);
#4868=ORIENTED_EDGE('',*,*,#3389,.T.);
#4869=ORIENTED_EDGE('',*,*,#3554,.F.);
#4870=ORIENTED_EDGE('',*,*,#3493,.F.);
#4871=ORIENTED_EDGE('',*,*,#3555,.F.);
#4872=ORIENTED_EDGE('',*,*,#3390,.F.);
#4873=ORIENTED_EDGE('',*,*,#3555,.T.);
#4874=ORIENTED_EDGE('',*,*,#3492,.F.);
#4875=ORIENTED_EDGE('',*,*,#3556,.T.);
#4876=ORIENTED_EDGE('',*,*,#3391,.T.);
#4877=ORIENTED_EDGE('',*,*,#3556,.F.);
#4878=ORIENTED_EDGE('',*,*,#3491,.F.);
#4879=ORIENTED_EDGE('',*,*,#3557,.F.);
#4880=ORIENTED_EDGE('',*,*,#3392,.F.);
#4881=ORIENTED_EDGE('',*,*,#3557,.T.);
#4882=ORIENTED_EDGE('',*,*,#3490,.F.);
#4883=ORIENTED_EDGE('',*,*,#3558,.T.);
#4884=ORIENTED_EDGE('',*,*,#3393,.T.);
#4885=ORIENTED_EDGE('',*,*,#3558,.F.);
#4886=ORIENTED_EDGE('',*,*,#3489,.F.);
#4887=ORIENTED_EDGE('',*,*,#3559,.F.);
#4888=ORIENTED_EDGE('',*,*,#3394,.F.);
#4889=ORIENTED_EDGE('',*,*,#3559,.T.);
#4890=ORIENTED_EDGE('',*,*,#3488,.F.);
#4891=ORIENTED_EDGE('',*,*,#3560,.T.);
#4892=ORIENTED_EDGE('',*,*,#3395,.T.);
#4893=ORIENTED_EDGE('',*,*,#3560,.F.);
#4894=ORIENTED_EDGE('',*,*,#3487,.F.);
#4895=ORIENTED_EDGE('',*,*,#3561,.F.);
#4896=ORIENTED_EDGE('',*,*,#3396,.F.);
#4897=ORIENTED_EDGE('',*,*,#3561,.T.);
#4898=ORIENTED_EDGE('',*,*,#3486,.F.);
#4899=ORIENTED_EDGE('',*,*,#3562,.T.);
#4900=ORIENTED_EDGE('',*,*,#3397,.T.);
#4901=ORIENTED_EDGE('',*,*,#3562,.F.);
#4902=ORIENTED_EDGE('',*,*,#3485,.F.);
#4903=ORIENTED_EDGE('',*,*,#3563,.F.);
#4904=ORIENTED_EDGE('',*,*,#3398,.F.);
#4905=ORIENTED_EDGE('',*,*,#3563,.T.);
#4906=ORIENTED_EDGE('',*,*,#3484,.F.);
#4907=ORIENTED_EDGE('',*,*,#3564,.T.);
#4908=ORIENTED_EDGE('',*,*,#3399,.T.);
#4909=ORIENTED_EDGE('',*,*,#3564,.F.);
#4910=ORIENTED_EDGE('',*,*,#3483,.F.);
#4911=ORIENTED_EDGE('',*,*,#3565,.F.);
#4912=ORIENTED_EDGE('',*,*,#3400,.F.);
#4913=ORIENTED_EDGE('',*,*,#3565,.T.);
#4914=ORIENTED_EDGE('',*,*,#3482,.F.);
#4915=ORIENTED_EDGE('',*,*,#3566,.T.);
#4916=ORIENTED_EDGE('',*,*,#3401,.T.);
#4917=ORIENTED_EDGE('',*,*,#3566,.F.);
#4918=ORIENTED_EDGE('',*,*,#3481,.F.);
#4919=ORIENTED_EDGE('',*,*,#3567,.F.);
#4920=ORIENTED_EDGE('',*,*,#3402,.F.);
#4921=ORIENTED_EDGE('',*,*,#3567,.T.);
#4922=ORIENTED_EDGE('',*,*,#3480,.F.);
#4923=ORIENTED_EDGE('',*,*,#3568,.T.);
#4924=ORIENTED_EDGE('',*,*,#3403,.T.);
#4925=ORIENTED_EDGE('',*,*,#3568,.F.);
#4926=ORIENTED_EDGE('',*,*,#3479,.F.);
#4927=ORIENTED_EDGE('',*,*,#3569,.F.);
#4928=ORIENTED_EDGE('',*,*,#3404,.F.);
#4929=ORIENTED_EDGE('',*,*,#3569,.T.);
#4930=ORIENTED_EDGE('',*,*,#3478,.F.);
#4931=ORIENTED_EDGE('',*,*,#3570,.T.);
#4932=ORIENTED_EDGE('',*,*,#3405,.T.);
#4933=ORIENTED_EDGE('',*,*,#3570,.F.);
#4934=ORIENTED_EDGE('',*,*,#3477,.F.);
#4935=ORIENTED_EDGE('',*,*,#3571,.F.);
#4936=ORIENTED_EDGE('',*,*,#3406,.F.);
#4937=ORIENTED_EDGE('',*,*,#3571,.T.);
#4938=ORIENTED_EDGE('',*,*,#3476,.F.);
#4939=ORIENTED_EDGE('',*,*,#3572,.T.);
#4940=ORIENTED_EDGE('',*,*,#3407,.T.);
#4941=ORIENTED_EDGE('',*,*,#3572,.F.);
#4942=ORIENTED_EDGE('',*,*,#3475,.F.);
#4943=ORIENTED_EDGE('',*,*,#3573,.F.);
#4944=ORIENTED_EDGE('',*,*,#3408,.F.);
#4945=ORIENTED_EDGE('',*,*,#3573,.T.);
#4946=ORIENTED_EDGE('',*,*,#3474,.F.);
#4947=ORIENTED_EDGE('',*,*,#3574,.T.);
#4948=ORIENTED_EDGE('',*,*,#3409,.T.);
#4949=ORIENTED_EDGE('',*,*,#3574,.F.);
#4950=ORIENTED_EDGE('',*,*,#3473,.F.);
#4951=ORIENTED_EDGE('',*,*,#3575,.F.);
#4952=ORIENTED_EDGE('',*,*,#3410,.F.);
#4953=ORIENTED_EDGE('',*,*,#3575,.T.);
#4954=ORIENTED_EDGE('',*,*,#3472,.F.);
#4955=ORIENTED_EDGE('',*,*,#3576,.T.);
#4956=ORIENTED_EDGE('',*,*,#3411,.T.);
#4957=ORIENTED_EDGE('',*,*,#3576,.F.);
#4958=ORIENTED_EDGE('',*,*,#3471,.F.);
#4959=ORIENTED_EDGE('',*,*,#3577,.F.);
#4960=ORIENTED_EDGE('',*,*,#3412,.F.);
#4961=ORIENTED_EDGE('',*,*,#3577,.T.);
#4962=ORIENTED_EDGE('',*,*,#3470,.F.);
#4963=ORIENTED_EDGE('',*,*,#3578,.T.);
#4964=ORIENTED_EDGE('',*,*,#3413,.T.);
#4965=ORIENTED_EDGE('',*,*,#3578,.F.);
#4966=ORIENTED_EDGE('',*,*,#3469,.F.);
#4967=ORIENTED_EDGE('',*,*,#3579,.F.);
#4968=ORIENTED_EDGE('',*,*,#3414,.F.);
#4969=ORIENTED_EDGE('',*,*,#3579,.T.);
#4970=ORIENTED_EDGE('',*,*,#3468,.F.);
#4971=ORIENTED_EDGE('',*,*,#3580,.T.);
#4972=ORIENTED_EDGE('',*,*,#3415,.T.);
#4973=ORIENTED_EDGE('',*,*,#3580,.F.);
#4974=ORIENTED_EDGE('',*,*,#3467,.F.);
#4975=ORIENTED_EDGE('',*,*,#3581,.F.);
#4976=ORIENTED_EDGE('',*,*,#3416,.F.);
#4977=ORIENTED_EDGE('',*,*,#3581,.T.);
#4978=ORIENTED_EDGE('',*,*,#3466,.F.);
#4979=ORIENTED_EDGE('',*,*,#3582,.T.);
#4980=ORIENTED_EDGE('',*,*,#3417,.T.);
#4981=ORIENTED_EDGE('',*,*,#3582,.F.);
#4982=ORIENTED_EDGE('',*,*,#3465,.F.);
#4983=ORIENTED_EDGE('',*,*,#3583,.F.);
#4984=ORIENTED_EDGE('',*,*,#3418,.F.);
#4985=ORIENTED_EDGE('',*,*,#3583,.T.);
#4986=ORIENTED_EDGE('',*,*,#3464,.F.);
#4987=ORIENTED_EDGE('',*,*,#3584,.T.);
#4988=ORIENTED_EDGE('',*,*,#3419,.T.);
#4989=ORIENTED_EDGE('',*,*,#3584,.F.);
#4990=ORIENTED_EDGE('',*,*,#3463,.F.);
#4991=ORIENTED_EDGE('',*,*,#3585,.F.);
#4992=ORIENTED_EDGE('',*,*,#3420,.F.);
#4993=ORIENTED_EDGE('',*,*,#3585,.T.);
#4994=ORIENTED_EDGE('',*,*,#3462,.F.);
#4995=ORIENTED_EDGE('',*,*,#3586,.T.);
#4996=ORIENTED_EDGE('',*,*,#3421,.T.);
#4997=ORIENTED_EDGE('',*,*,#3586,.F.);
#4998=ORIENTED_EDGE('',*,*,#3461,.F.);
#4999=ORIENTED_EDGE('',*,*,#3587,.F.);
#5000=ORIENTED_EDGE('',*,*,#3422,.F.);
#5001=ORIENTED_EDGE('',*,*,#3587,.T.);
#5002=ORIENTED_EDGE('',*,*,#3460,.F.);
#5003=ORIENTED_EDGE('',*,*,#3588,.T.);
#5004=ORIENTED_EDGE('',*,*,#3423,.T.);
#5005=ORIENTED_EDGE('',*,*,#3588,.F.);
#5006=ORIENTED_EDGE('',*,*,#3459,.F.);
#5007=ORIENTED_EDGE('',*,*,#3589,.F.);
#5008=ORIENTED_EDGE('',*,*,#3424,.F.);
#5009=ORIENTED_EDGE('',*,*,#3589,.T.);
#5010=ORIENTED_EDGE('',*,*,#3458,.F.);
#5011=ORIENTED_EDGE('',*,*,#3590,.T.);
#5012=ORIENTED_EDGE('',*,*,#3425,.T.);
#5013=ORIENTED_EDGE('',*,*,#3590,.F.);
#5014=ORIENTED_EDGE('',*,*,#3457,.F.);
#5015=ORIENTED_EDGE('',*,*,#3591,.F.);
#5016=ORIENTED_EDGE('',*,*,#3426,.F.);
#5017=ORIENTED_EDGE('',*,*,#3591,.T.);
#5018=ORIENTED_EDGE('',*,*,#3456,.F.);
#5019=ORIENTED_EDGE('',*,*,#3592,.T.);
#5020=ORIENTED_EDGE('',*,*,#3427,.T.);
#5021=ORIENTED_EDGE('',*,*,#3592,.F.);
#5022=ORIENTED_EDGE('',*,*,#3455,.F.);
#5023=ORIENTED_EDGE('',*,*,#3593,.F.);
#5024=ORIENTED_EDGE('',*,*,#3428,.F.);
#5025=ORIENTED_EDGE('',*,*,#3593,.T.);
#5026=ORIENTED_EDGE('',*,*,#3454,.F.);
#5027=ORIENTED_EDGE('',*,*,#3594,.T.);
#5028=ORIENTED_EDGE('',*,*,#3429,.T.);
#5029=ORIENTED_EDGE('',*,*,#3594,.F.);
#5030=ORIENTED_EDGE('',*,*,#3453,.F.);
#5031=ORIENTED_EDGE('',*,*,#3595,.F.);
#5032=ORIENTED_EDGE('',*,*,#3430,.F.);
#5033=ORIENTED_EDGE('',*,*,#3595,.T.);
#5034=ORIENTED_EDGE('',*,*,#3452,.F.);
#5035=ORIENTED_EDGE('',*,*,#3596,.T.);
#5036=ORIENTED_EDGE('',*,*,#3431,.T.);
#5037=ORIENTED_EDGE('',*,*,#3596,.F.);
#5038=ORIENTED_EDGE('',*,*,#3451,.F.);
#5039=ORIENTED_EDGE('',*,*,#3597,.F.);
#5040=ORIENTED_EDGE('',*,*,#3432,.F.);
#5041=ORIENTED_EDGE('',*,*,#3597,.T.);
#5042=ORIENTED_EDGE('',*,*,#3450,.F.);
#5043=ORIENTED_EDGE('',*,*,#3598,.T.);
#5044=ORIENTED_EDGE('',*,*,#3433,.T.);
#5045=ORIENTED_EDGE('',*,*,#3598,.F.);
#5046=ORIENTED_EDGE('',*,*,#3449,.F.);
#5047=ORIENTED_EDGE('',*,*,#3599,.F.);
#5048=ORIENTED_EDGE('',*,*,#3434,.F.);
#5049=ORIENTED_EDGE('',*,*,#3599,.T.);
#5050=ORIENTED_EDGE('',*,*,#3448,.F.);
#5051=ORIENTED_EDGE('',*,*,#3600,.T.);
#5052=ORIENTED_EDGE('',*,*,#3435,.T.);
#5053=ORIENTED_EDGE('',*,*,#3601,.F.);
#5054=ORIENTED_EDGE('',*,*,#3436,.F.);
#5055=ORIENTED_EDGE('',*,*,#3600,.F.);
#5056=ORIENTED_EDGE('',*,*,#3447,.F.);
#5057=ORIENTED_EDGE('',*,*,#3524,.T.);
#5058=ORIENTED_EDGE('',*,*,#3439,.T.);
#5059=ORIENTED_EDGE('',*,*,#3602,.T.);
#5060=ORIENTED_EDGE('',*,*,#3444,.F.);
#5061=ORIENTED_EDGE('',*,*,#3603,.F.);
#5062=ORIENTED_EDGE('',*,*,#3445,.F.);
#5063=ORIENTED_EDGE('',*,*,#3602,.F.);
#5064=ORIENTED_EDGE('',*,*,#3438,.F.);
#5065=ORIENTED_EDGE('',*,*,#3601,.T.);
#5066=ORIENTED_EDGE('',*,*,#3446,.F.);
#5067=ORIENTED_EDGE('',*,*,#3603,.T.);
#5068=ORIENTED_EDGE('',*,*,#3437,.T.);
#5069=ORIENTED_EDGE('',*,*,#3604,.F.);
#5070=ORIENTED_EDGE('',*,*,#3605,.F.);
#5071=ORIENTED_EDGE('',*,*,#3606,.F.);
#5072=ORIENTED_EDGE('',*,*,#3607,.F.);
#5073=ORIENTED_EDGE('',*,*,#3608,.F.);
#5074=ORIENTED_EDGE('',*,*,#3609,.F.);
#5075=ORIENTED_EDGE('',*,*,#3610,.F.);
#5076=ORIENTED_EDGE('',*,*,#3611,.F.);
#5077=ORIENTED_EDGE('',*,*,#3608,.T.);
#5078=ORIENTED_EDGE('',*,*,#3612,.T.);
#5079=ORIENTED_EDGE('',*,*,#3613,.T.);
#5080=ORIENTED_EDGE('',*,*,#3614,.T.);
#5081=ORIENTED_EDGE('',*,*,#3607,.T.);
#5082=ORIENTED_EDGE('',*,*,#3615,.F.);
#5083=ORIENTED_EDGE('',*,*,#3616,.T.);
#5084=ORIENTED_EDGE('',*,*,#3612,.F.);
#5085=ORIENTED_EDGE('',*,*,#3606,.T.);
#5086=ORIENTED_EDGE('',*,*,#3617,.T.);
#5087=ORIENTED_EDGE('',*,*,#3618,.T.);
#5088=ORIENTED_EDGE('',*,*,#3615,.T.);
#5089=ORIENTED_EDGE('',*,*,#3605,.T.);
#5090=ORIENTED_EDGE('',*,*,#3619,.F.);
#5091=ORIENTED_EDGE('',*,*,#3620,.T.);
#5092=ORIENTED_EDGE('',*,*,#3617,.F.);
#5093=ORIENTED_EDGE('',*,*,#3613,.F.);
#5094=ORIENTED_EDGE('',*,*,#3616,.F.);
#5095=ORIENTED_EDGE('',*,*,#3618,.F.);
#5096=ORIENTED_EDGE('',*,*,#3620,.F.);
#5097=ORIENTED_EDGE('',*,*,#3621,.F.);
#5098=ORIENTED_EDGE('',*,*,#3622,.F.);
#5099=ORIENTED_EDGE('',*,*,#3623,.F.);
#5100=ORIENTED_EDGE('',*,*,#3624,.F.);
#5101=ORIENTED_EDGE('',*,*,#3604,.T.);
#5102=ORIENTED_EDGE('',*,*,#3625,.T.);
#5103=ORIENTED_EDGE('',*,*,#3621,.T.);
#5104=ORIENTED_EDGE('',*,*,#3619,.T.);
#5105=ORIENTED_EDGE('',*,*,#3611,.T.);
#5106=ORIENTED_EDGE('',*,*,#3626,.F.);
#5107=ORIENTED_EDGE('',*,*,#3622,.T.);
#5108=ORIENTED_EDGE('',*,*,#3625,.F.);
#5109=ORIENTED_EDGE('',*,*,#3610,.T.);
#5110=ORIENTED_EDGE('',*,*,#3627,.T.);
#5111=ORIENTED_EDGE('',*,*,#3623,.T.);
#5112=ORIENTED_EDGE('',*,*,#3626,.T.);
#5113=ORIENTED_EDGE('',*,*,#3609,.T.);
#5114=ORIENTED_EDGE('',*,*,#3614,.F.);
#5115=ORIENTED_EDGE('',*,*,#3624,.T.);
#5116=ORIENTED_EDGE('',*,*,#3627,.F.);
#5117=ORIENTED_EDGE('',*,*,#3628,.F.);
#5118=ORIENTED_EDGE('',*,*,#3629,.T.);
#5119=ORIENTED_EDGE('',*,*,#3630,.T.);
#5120=ORIENTED_EDGE('',*,*,#3631,.F.);
#5121=ORIENTED_EDGE('',*,*,#3632,.F.);
#5122=ORIENTED_EDGE('',*,*,#3633,.T.);
#5123=ORIENTED_EDGE('',*,*,#3634,.T.);
#5124=ORIENTED_EDGE('',*,*,#3629,.F.);
#5125=ORIENTED_EDGE('',*,*,#3635,.F.);
#5126=ORIENTED_EDGE('',*,*,#3636,.T.);
#5127=ORIENTED_EDGE('',*,*,#3637,.T.);
#5128=ORIENTED_EDGE('',*,*,#3633,.F.);
#5129=ORIENTED_EDGE('',*,*,#3638,.F.);
#5130=ORIENTED_EDGE('',*,*,#3639,.T.);
#5131=ORIENTED_EDGE('',*,*,#3640,.T.);
#5132=ORIENTED_EDGE('',*,*,#3636,.F.);
#5133=ORIENTED_EDGE('',*,*,#3641,.F.);
#5134=ORIENTED_EDGE('',*,*,#3642,.T.);
#5135=ORIENTED_EDGE('',*,*,#3643,.T.);
#5136=ORIENTED_EDGE('',*,*,#3639,.F.);
#5137=ORIENTED_EDGE('',*,*,#3644,.F.);
#5138=ORIENTED_EDGE('',*,*,#3631,.T.);
#5139=ORIENTED_EDGE('',*,*,#3645,.T.);
#5140=ORIENTED_EDGE('',*,*,#3642,.F.);
#5141=ORIENTED_EDGE('',*,*,#3645,.F.);
#5142=ORIENTED_EDGE('',*,*,#3630,.F.);
#5143=ORIENTED_EDGE('',*,*,#3634,.F.);
#5144=ORIENTED_EDGE('',*,*,#3637,.F.);
#5145=ORIENTED_EDGE('',*,*,#3640,.F.);
#5146=ORIENTED_EDGE('',*,*,#3643,.F.);
#5147=ORIENTED_EDGE('',*,*,#3646,.F.);
#5148=ORIENTED_EDGE('',*,*,#3628,.T.);
#5149=ORIENTED_EDGE('',*,*,#3644,.T.);
#5150=ORIENTED_EDGE('',*,*,#3641,.T.);
#5151=ORIENTED_EDGE('',*,*,#3638,.T.);
#5152=ORIENTED_EDGE('',*,*,#3635,.T.);
#5153=ORIENTED_EDGE('',*,*,#3632,.T.);
#5154=ORIENTED_EDGE('',*,*,#3647,.F.);
#5155=ORIENTED_EDGE('',*,*,#3648,.T.);
#5156=ORIENTED_EDGE('',*,*,#3646,.T.);
#5157=ORIENTED_EDGE('',*,*,#3648,.F.);
#5158=ORIENTED_EDGE('',*,*,#3649,.F.);
#5159=ORIENTED_EDGE('',*,*,#3650,.T.);
#5160=ORIENTED_EDGE('',*,*,#3647,.T.);
#5161=ORIENTED_EDGE('',*,*,#3650,.F.);
#5162=ORIENTED_EDGE('',*,*,#3651,.F.);
#5163=ORIENTED_EDGE('',*,*,#3652,.T.);
#5164=ORIENTED_EDGE('',*,*,#3649,.T.);
#5165=ORIENTED_EDGE('',*,*,#3652,.F.);
#5166=ORIENTED_EDGE('',*,*,#3651,.T.);
#5167=CYLINDRICAL_SURFACE('',#5928,0.25);
#5168=CYLINDRICAL_SURFACE('',#5931,0.25);
#5169=CYLINDRICAL_SURFACE('',#5934,0.25);
#5170=CYLINDRICAL_SURFACE('',#5937,0.25);
#5171=CYLINDRICAL_SURFACE('',#5947,0.165);
#5172=CYLINDRICAL_SURFACE('',#5951,0.165);
#5173=CYLINDRICAL_SURFACE('',#5955,0.165);
#5174=CYLINDRICAL_SURFACE('',#5959,0.165);
#5175=CYLINDRICAL_SURFACE('',#5963,0.165);
#5176=CYLINDRICAL_SURFACE('',#5967,0.165);
#5177=CYLINDRICAL_SURFACE('',#5971,0.165);
#5178=CYLINDRICAL_SURFACE('',#5975,0.165);
#5179=CYLINDRICAL_SURFACE('',#5979,0.33);
#5180=CYLINDRICAL_SURFACE('',#5982,0.33);
#5181=CYLINDRICAL_SURFACE('',#5985,0.33);
#5182=CYLINDRICAL_SURFACE('',#5988,0.33);
#5183=CYLINDRICAL_SURFACE('',#6017,2.35);
#5184=CYLINDRICAL_SURFACE('',#6020,3.5);
#5185=CYLINDRICAL_SURFACE('',#6026,1.75);
#5186=CYLINDRICAL_SURFACE('',#6029,2.34);
#5187=CYLINDRICAL_SURFACE('',#6035,0.225);
#5188=CYLINDRICAL_SURFACE('',#6038,0.225);
#5189=CYLINDRICAL_SURFACE('',#6041,0.225);
#5190=CYLINDRICAL_SURFACE('',#6044,0.225);
#5191=CYLINDRICAL_SURFACE('',#6047,2.34);
#5192=CYLINDRICAL_SURFACE('',#6052,1.8);
#5193=CYLINDRICAL_SURFACE('',#6057,1.6);
#5194=CYLINDRICAL_SURFACE('',#6058,3.5);
#5195=CYLINDRICAL_SURFACE('',#6064,1.);
#5196=CYLINDRICAL_SURFACE('',#6067,1.8);
#5197=CYLINDRICAL_SURFACE('',#6073,0.225);
#5198=CYLINDRICAL_SURFACE('',#6076,0.225);
#5199=CYLINDRICAL_SURFACE('',#6079,0.225);
#5200=CYLINDRICAL_SURFACE('',#6082,0.225);
#5201=CYLINDRICAL_SURFACE('',#6085,2.34);
#5202=CYLINDRICAL_SURFACE('',#6090,1.8);
#5203=CYLINDRICAL_SURFACE('',#6092,3.5);
#5204=CYLINDRICAL_SURFACE('',#6119,1.63531);
#5205=CYLINDRICAL_SURFACE('',#6121,1.);
#5206=CYLINDRICAL_SURFACE('',#6127,1.63531);
#5207=CYLINDRICAL_SURFACE('',#6139,1.71469);
#5208=CYLINDRICAL_SURFACE('',#6146,2.35);
#5209=CYLINDRICAL_SURFACE('',#6151,1.71469);
#5210=CYLINDRICAL_SURFACE('',#6173,1.706752);
#5211=CYLINDRICAL_SURFACE('',#6213,1.643248);
#5212=CYLINDRICAL_SURFACE('',#6227,1.70469);
#5213=CYLINDRICAL_SURFACE('',#6231,1.65031);
#5214=CYLINDRICAL_SURFACE('',#6235,1.70469);
#5215=CYLINDRICAL_SURFACE('',#6239,1.65031);
#5216=CYLINDRICAL_SURFACE('',#6250,0.5);
#5217=CYLINDRICAL_SURFACE('',#6258,0.2942);
#5218=CYLINDRICAL_SURFACE('',#6276,0.35);
#5219=CYLINDRICAL_SURFACE('',#6284,0.1954);
#5220=CYLINDRICAL_SURFACE('',#6328,0.6);
#5221=CYLINDRICAL_SURFACE('',#6338,1.2);
#5222=CYLINDRICAL_SURFACE('',#6339,1.);
#5223=CYLINDRICAL_SURFACE('',#6341,1.);
#5224=CYLINDRICAL_SURFACE('',#6346,1.01);
#5225=CYLINDRICAL_SURFACE('',#6349,1.35);
#5226=CYLINDRICAL_SURFACE('',#6357,0.21);
#5227=CYLINDRICAL_SURFACE('',#6361,1.005);
#5228=CYLINDRICAL_SURFACE('',#6364,1.5);
#5229=CYLINDRICAL_SURFACE('',#6372,0.21);
#5230=CYLINDRICAL_SURFACE('',#6376,0.605);
#5231=CYLINDRICAL_SURFACE('',#6379,1.2);
#5232=CYLINDRICAL_SURFACE('',#6392,0.6);
#5233=CYLINDRICAL_SURFACE('',#6394,0.125);
#5234=CYLINDRICAL_SURFACE('',#6395,0.125);
#5235=CYLINDRICAL_SURFACE('',#6396,1.);
#5236=CYLINDRICAL_SURFACE('',#6399,0.125);
#5237=CYLINDRICAL_SURFACE('',#6400,0.125);
#5238=CYLINDRICAL_SURFACE('',#6484,1.4);
#5239=CYLINDRICAL_SURFACE('',#6569,1.4);
#5240=CYLINDRICAL_SURFACE('',#6570,0.0555000000000001);
#5241=CYLINDRICAL_SURFACE('',#6571,1.24783954473516);
#5242=CYLINDRICAL_SURFACE('',#6572,0.0555000000000001);
#5243=CYLINDRICAL_SURFACE('',#6573,1.24783954473516);
#5244=CYLINDRICAL_SURFACE('',#6574,0.0555000000000001);
#5245=CYLINDRICAL_SURFACE('',#6575,1.24783954473516);
#5246=CYLINDRICAL_SURFACE('',#6576,0.0555000000000001);
#5247=CYLINDRICAL_SURFACE('',#6577,1.24783954473516);
#5248=CYLINDRICAL_SURFACE('',#6578,0.0555000000000001);
#5249=CYLINDRICAL_SURFACE('',#6579,1.24783954473516);
#5250=CYLINDRICAL_SURFACE('',#6580,0.0555000000000001);
#5251=CYLINDRICAL_SURFACE('',#6581,1.24783954473516);
#5252=CYLINDRICAL_SURFACE('',#6582,0.0555000000000001);
#5253=CYLINDRICAL_SURFACE('',#6583,1.24783954473516);
#5254=CYLINDRICAL_SURFACE('',#6584,0.0555000000000001);
#5255=CYLINDRICAL_SURFACE('',#6585,1.24783954473516);
#5256=CYLINDRICAL_SURFACE('',#6586,0.0555000000000001);
#5257=CYLINDRICAL_SURFACE('',#6587,1.24783954473516);
#5258=CYLINDRICAL_SURFACE('',#6588,0.0555000000000001);
#5259=CYLINDRICAL_SURFACE('',#6589,1.24783954473516);
#5260=CYLINDRICAL_SURFACE('',#6590,0.0555000000000001);
#5261=CYLINDRICAL_SURFACE('',#6591,1.24783954473516);
#5262=CYLINDRICAL_SURFACE('',#6592,0.0555000000000001);
#5263=CYLINDRICAL_SURFACE('',#6593,1.24783954473516);
#5264=CYLINDRICAL_SURFACE('',#6594,0.0555000000000001);
#5265=CYLINDRICAL_SURFACE('',#6595,1.24783954473516);
#5266=CYLINDRICAL_SURFACE('',#6596,0.0555000000000001);
#5267=CYLINDRICAL_SURFACE('',#6597,1.24783954473516);
#5268=CYLINDRICAL_SURFACE('',#6598,0.0555000000000001);
#5269=CYLINDRICAL_SURFACE('',#6599,1.24783954473516);
#5270=CYLINDRICAL_SURFACE('',#6600,0.0555000000000001);
#5271=CYLINDRICAL_SURFACE('',#6601,1.24783954473516);
#5272=CYLINDRICAL_SURFACE('',#6602,0.0555000000000001);
#5273=CYLINDRICAL_SURFACE('',#6603,1.24783954473516);
#5274=CYLINDRICAL_SURFACE('',#6604,0.0555000000000001);
#5275=CYLINDRICAL_SURFACE('',#6605,1.24783954473516);
#5276=CYLINDRICAL_SURFACE('',#6606,0.0555000000000001);
#5277=CYLINDRICAL_SURFACE('',#6607,1.24783954473516);
#5278=CYLINDRICAL_SURFACE('',#6608,0.0555000000000001);
#5279=CYLINDRICAL_SURFACE('',#6609,1.24783954473516);
#5280=CYLINDRICAL_SURFACE('',#6610,0.0555000000000001);
#5281=CYLINDRICAL_SURFACE('',#6611,1.24783954473516);
#5282=CYLINDRICAL_SURFACE('',#6612,0.0555000000000001);
#5283=CYLINDRICAL_SURFACE('',#6613,1.24783954473516);
#5284=CYLINDRICAL_SURFACE('',#6614,0.0555000000000001);
#5285=CYLINDRICAL_SURFACE('',#6615,1.24783954473516);
#5286=CYLINDRICAL_SURFACE('',#6616,0.0555000000000001);
#5287=CYLINDRICAL_SURFACE('',#6617,1.24783954473516);
#5288=CYLINDRICAL_SURFACE('',#6618,0.0555000000000001);
#5289=CYLINDRICAL_SURFACE('',#6619,1.24783954473516);
#5290=CYLINDRICAL_SURFACE('',#6620,0.0555000000000001);
#5291=CYLINDRICAL_SURFACE('',#6621,1.24783954473516);
#5292=CYLINDRICAL_SURFACE('',#6622,0.0555000000000001);
#5293=CYLINDRICAL_SURFACE('',#6623,1.24783954473516);
#5294=CYLINDRICAL_SURFACE('',#6624,0.0555000000000001);
#5295=CYLINDRICAL_SURFACE('',#6625,1.24783954473516);
#5296=CYLINDRICAL_SURFACE('',#6626,0.0555000000000001);
#5297=CYLINDRICAL_SURFACE('',#6627,1.24783954473516);
#5298=CYLINDRICAL_SURFACE('',#6628,0.0555000000000001);
#5299=CYLINDRICAL_SURFACE('',#6629,1.24783954473516);
#5300=CYLINDRICAL_SURFACE('',#6630,0.0555000000000001);
#5301=CYLINDRICAL_SURFACE('',#6631,1.24783954473516);
#5302=CYLINDRICAL_SURFACE('',#6632,0.0555000000000001);
#5303=CYLINDRICAL_SURFACE('',#6633,1.24783954473516);
#5304=CYLINDRICAL_SURFACE('',#6634,0.0555000000000001);
#5305=CYLINDRICAL_SURFACE('',#6635,1.24783954473516);
#5306=CYLINDRICAL_SURFACE('',#6636,0.0555000000000001);
#5307=CYLINDRICAL_SURFACE('',#6637,1.24783954473516);
#5308=CYLINDRICAL_SURFACE('',#6638,0.0555000000000001);
#5309=CYLINDRICAL_SURFACE('',#6639,1.24783954473516);
#5310=CYLINDRICAL_SURFACE('',#6640,0.0555000000000001);
#5311=CYLINDRICAL_SURFACE('',#6641,1.24783954473516);
#5312=CYLINDRICAL_SURFACE('',#6642,0.0555000000000001);
#5313=CYLINDRICAL_SURFACE('',#6643,1.24783954473516);
#5314=CYLINDRICAL_SURFACE('',#6644,0.0555000000000001);
#5315=CYLINDRICAL_SURFACE('',#6645,1.24783954473516);
#5316=CYLINDRICAL_SURFACE('',#6646,0.0555000000000001);
#5317=CYLINDRICAL_SURFACE('',#6647,1.24783954473516);
#5318=CYLINDRICAL_SURFACE('',#6648,0.0555000000000001);
#5319=CYLINDRICAL_SURFACE('',#6649,1.24783954473516);
#5320=CYLINDRICAL_SURFACE('',#6673,0.24505);
#5321=ADVANCED_FACE('',(#577),#5167,.F.);
#5322=ADVANCED_FACE('',(#578),#5168,.F.);
#5323=ADVANCED_FACE('',(#579),#5169,.F.);
#5324=ADVANCED_FACE('',(#580),#5170,.F.);
#5325=ADVANCED_FACE('',(#581),#434,.T.);
#5326=ADVANCED_FACE('',(#582),#435,.T.);
#5327=ADVANCED_FACE('',(#583),#436,.T.);
#5328=ADVANCED_FACE('',(#584),#437,.T.);
#5329=ADVANCED_FACE('',(#585,#341,#342,#343,#344),#438,.T.);
#5330=ADVANCED_FACE('',(#586,#345,#346,#347,#348),#439,.F.);
#5331=ADVANCED_FACE('',(#587),#5171,.F.);
#5332=ADVANCED_FACE('',(#588),#440,.T.);
#5333=ADVANCED_FACE('',(#589),#5172,.F.);
#5334=ADVANCED_FACE('',(#590),#441,.T.);
#5335=ADVANCED_FACE('',(#591),#5173,.F.);
#5336=ADVANCED_FACE('',(#592),#442,.T.);
#5337=ADVANCED_FACE('',(#593),#5174,.F.);
#5338=ADVANCED_FACE('',(#594),#443,.T.);
#5339=ADVANCED_FACE('',(#595),#5175,.F.);
#5340=ADVANCED_FACE('',(#596),#444,.F.);
#5341=ADVANCED_FACE('',(#597),#5176,.F.);
#5342=ADVANCED_FACE('',(#598),#445,.F.);
#5343=ADVANCED_FACE('',(#599),#5177,.F.);
#5344=ADVANCED_FACE('',(#600),#446,.F.);
#5345=ADVANCED_FACE('',(#601),#5178,.F.);
#5346=ADVANCED_FACE('',(#602),#447,.F.);
#5347=ADVANCED_FACE('',(#603),#5179,.F.);
#5348=ADVANCED_FACE('',(#604),#5180,.F.);
#5349=ADVANCED_FACE('',(#605),#5181,.F.);
#5350=ADVANCED_FACE('',(#606),#5182,.F.);
#5351=ADVANCED_FACE('',(#607),#448,.T.);
#5352=ADVANCED_FACE('',(#608),#449,.T.);
#5353=ADVANCED_FACE('',(#609),#450,.F.);
#5354=ADVANCED_FACE('',(#610),#451,.F.);
#5355=ADVANCED_FACE('',(#611,#349),#452,.T.);
#5356=ADVANCED_FACE('',(#612,#350),#453,.T.);
#5357=ADVANCED_FACE('',(#613),#454,.T.);
#5358=ADVANCED_FACE('',(#614,#351,#352),#455,.T.);
#5359=ADVANCED_FACE('',(#615),#456,.T.);
#5360=ADVANCED_FACE('',(#616),#457,.T.);
#5361=ADVANCED_FACE('',(#617),#458,.T.);
#5362=ADVANCED_FACE('',(#618),#459,.F.);
#5363=ADVANCED_FACE('',(#619),#460,.F.);
#5364=ADVANCED_FACE('',(#620,#353),#461,.T.);
#5365=ADVANCED_FACE('',(#621,#354),#462,.T.);
#5366=ADVANCED_FACE('',(#622),#463,.T.);
#5367=ADVANCED_FACE('',(#623,#355,#356),#464,.T.);
#5368=ADVANCED_FACE('',(#624),#465,.T.);
#5369=ADVANCED_FACE('',(#625),#5183,.F.);
#5370=ADVANCED_FACE('',(#626,#357,#358),#5184,.T.);
#5371=ADVANCED_FACE('',(#627,#359,#360,#361,#362,#363),#466,.T.);
#5372=ADVANCED_FACE('',(#628,#364,#365,#366,#367,#368),#467,.F.);
#5373=ADVANCED_FACE('',(#629),#5185,.F.);
#5374=ADVANCED_FACE('',(#630),#5186,.T.);
#5375=ADVANCED_FACE('',(#631,#369),#468,.T.);
#5376=ADVANCED_FACE('',(#632,#370),#469,.F.);
#5377=ADVANCED_FACE('',(#633),#5187,.F.);
#5378=ADVANCED_FACE('',(#634),#5188,.F.);
#5379=ADVANCED_FACE('',(#635),#5189,.F.);
#5380=ADVANCED_FACE('',(#636),#5190,.F.);
#5381=ADVANCED_FACE('',(#637),#5191,.T.);
#5382=ADVANCED_FACE('',(#638,#371),#470,.T.);
#5383=ADVANCED_FACE('',(#639),#5192,.F.);
#5384=ADVANCED_FACE('',(#640,#372),#471,.F.);
#5385=ADVANCED_FACE('',(#641),#5193,.F.);
#5386=ADVANCED_FACE('',(#642),#5194,.T.);
#5387=ADVANCED_FACE('',(#643,#373,#374,#375,#376,#377),#472,.T.);
#5388=ADVANCED_FACE('',(#644,#378,#379,#380,#381,#382),#473,.F.);
#5389=ADVANCED_FACE('',(#645),#5195,.F.);
#5390=ADVANCED_FACE('',(#646),#5196,.T.);
#5391=ADVANCED_FACE('',(#647,#383),#474,.T.);
#5392=ADVANCED_FACE('',(#648,#384),#475,.F.);
#5393=ADVANCED_FACE('',(#649),#5197,.F.);
#5394=ADVANCED_FACE('',(#650),#5198,.F.);
#5395=ADVANCED_FACE('',(#651),#5199,.F.);
#5396=ADVANCED_FACE('',(#652),#5200,.F.);
#5397=ADVANCED_FACE('',(#653),#5201,.T.);
#5398=ADVANCED_FACE('',(#654,#385),#476,.F.);
#5399=ADVANCED_FACE('',(#655),#5202,.F.);
#5400=ADVANCED_FACE('',(#656),#5203,.T.);
#5401=ADVANCED_FACE('',(#657,#386,#387,#388,#389,#390),#477,.T.);
#5402=ADVANCED_FACE('',(#658,#391,#392,#393,#394,#395),#478,.F.);
#5403=ADVANCED_FACE('',(#659),#479,.T.);
#5404=ADVANCED_FACE('',(#660),#480,.T.);
#5405=ADVANCED_FACE('',(#661),#481,.T.);
#5406=ADVANCED_FACE('',(#662),#482,.T.);
#5407=ADVANCED_FACE('',(#663),#483,.T.);
#5408=ADVANCED_FACE('',(#664),#484,.F.);
#5409=ADVANCED_FACE('',(#665),#485,.T.);
#5410=ADVANCED_FACE('',(#666),#486,.T.);
#5411=ADVANCED_FACE('',(#667),#487,.T.);
#5412=ADVANCED_FACE('',(#668),#488,.T.);
#5413=ADVANCED_FACE('',(#669),#489,.T.);
#5414=ADVANCED_FACE('',(#670),#490,.F.);
#5415=ADVANCED_FACE('',(#671),#237,.F.);
#5416=ADVANCED_FACE('',(#672),#5204,.T.);
#5417=ADVANCED_FACE('',(#673),#5205,.F.);
#5418=ADVANCED_FACE('',(#674),#223,.F.);
#5419=ADVANCED_FACE('',(#675,#396),#491,.T.);
#5420=ADVANCED_FACE('',(#676),#5206,.T.);
#5421=ADVANCED_FACE('',(#677,#397),#492,.T.);
#5422=ADVANCED_FACE('',(#678),#224,.F.);
#5423=ADVANCED_FACE('',(#679),#238,.F.);
#5424=ADVANCED_FACE('',(#680),#5207,.F.);
#5425=ADVANCED_FACE('',(#681,#398),#493,.T.);
#5426=ADVANCED_FACE('',(#682),#225,.T.);
#5427=ADVANCED_FACE('',(#683),#5208,.T.);
#5428=ADVANCED_FACE('',(#684),#226,.T.);
#5429=ADVANCED_FACE('',(#685,#399),#494,.T.);
#5430=ADVANCED_FACE('',(#686),#5209,.F.);
#5431=ADVANCED_FACE('',(#687),#207,.T.);
#5432=ADVANCED_FACE('',(#688),#208,.T.);
#5433=ADVANCED_FACE('',(#689),#209,.T.);
#5434=ADVANCED_FACE('',(#690),#210,.T.);
#5435=ADVANCED_FACE('',(#691),#211,.T.);
#5436=ADVANCED_FACE('',(#692),#212,.T.);
#5437=ADVANCED_FACE('',(#693),#213,.T.);
#5438=ADVANCED_FACE('',(#694),#214,.T.);
#5439=ADVANCED_FACE('',(#695),#215,.F.);
#5440=ADVANCED_FACE('',(#696),#5210,.T.);
#5441=ADVANCED_FACE('',(#697),#495,.T.);
#5442=ADVANCED_FACE('',(#698),#216,.F.);
#5443=ADVANCED_FACE('',(#699),#496,.T.);
#5444=ADVANCED_FACE('',(#700),#217,.F.);
#5445=ADVANCED_FACE('',(#701),#497,.T.);
#5446=ADVANCED_FACE('',(#702),#218,.F.);
#5447=ADVANCED_FACE('',(#703),#498,.T.);
#5448=ADVANCED_FACE('',(#704),#219,.F.);
#5449=ADVANCED_FACE('',(#705),#499,.T.);
#5450=ADVANCED_FACE('',(#706),#220,.F.);
#5451=ADVANCED_FACE('',(#707),#500,.T.);
#5452=ADVANCED_FACE('',(#708),#221,.F.);
#5453=ADVANCED_FACE('',(#709),#5211,.F.);
#5454=ADVANCED_FACE('',(#710),#501,.T.);
#5455=ADVANCED_FACE('',(#711),#222,.F.);
#5456=ADVANCED_FACE('',(#712,#400),#502,.T.);
#5457=ADVANCED_FACE('',(#713),#503,.T.);
#5458=ADVANCED_FACE('',(#714,#401),#504,.T.);
#5459=ADVANCED_FACE('',(#715),#5212,.T.);
#5460=ADVANCED_FACE('',(#716,#402),#505,.T.);
#5461=ADVANCED_FACE('',(#717),#5213,.F.);
#5462=ADVANCED_FACE('',(#718,#403),#506,.T.);
#5463=ADVANCED_FACE('',(#719),#5214,.T.);
#5464=ADVANCED_FACE('',(#720,#404),#507,.T.);
#5465=ADVANCED_FACE('',(#721),#5215,.F.);
#5466=ADVANCED_FACE('',(#722),#508,.T.);
#5467=ADVANCED_FACE('',(#723),#227,.T.);
#5468=ADVANCED_FACE('',(#724),#5216,.T.);
#5469=ADVANCED_FACE('',(#725),#228,.T.);
#5470=ADVANCED_FACE('',(#726,#405),#509,.T.);
#5471=ADVANCED_FACE('',(#727),#229,.T.);
#5472=ADVANCED_FACE('',(#728),#5217,.T.);
#5473=ADVANCED_FACE('',(#729),#230,.T.);
#5474=ADVANCED_FACE('',(#730),#510,.T.);
#5475=ADVANCED_FACE('',(#731),#511,.F.);
#5476=ADVANCED_FACE('',(#732),#512,.F.);
#5477=ADVANCED_FACE('',(#733),#513,.F.);
#5478=ADVANCED_FACE('',(#734),#514,.F.);
#5479=ADVANCED_FACE('',(#735),#515,.F.);
#5480=ADVANCED_FACE('',(#736),#516,.F.);
#5481=ADVANCED_FACE('',(#737),#517,.F.);
#5482=ADVANCED_FACE('',(#738),#518,.F.);
#5483=ADVANCED_FACE('',(#739),#519,.T.);
#5484=ADVANCED_FACE('',(#740),#231,.T.);
#5485=ADVANCED_FACE('',(#741),#5218,.T.);
#5486=ADVANCED_FACE('',(#742),#232,.T.);
#5487=ADVANCED_FACE('',(#743,#406),#520,.T.);
#5488=ADVANCED_FACE('',(#744),#233,.T.);
#5489=ADVANCED_FACE('',(#745),#5219,.T.);
#5490=ADVANCED_FACE('',(#746),#234,.T.);
#5491=ADVANCED_FACE('',(#747),#521,.T.);
#5492=ADVANCED_FACE('',(#748),#522,.F.);
#5493=ADVANCED_FACE('',(#749),#523,.F.);
#5494=ADVANCED_FACE('',(#750),#524,.F.);
#5495=ADVANCED_FACE('',(#751),#525,.F.);
#5496=ADVANCED_FACE('',(#752),#526,.F.);
#5497=ADVANCED_FACE('',(#753),#527,.F.);
#5498=ADVANCED_FACE('',(#754),#528,.F.);
#5499=ADVANCED_FACE('',(#755),#529,.F.);
#5500=ADVANCED_FACE('',(#756),#530,.F.);
#5501=ADVANCED_FACE('',(#757),#531,.T.);
#5502=ADVANCED_FACE('',(#758),#532,.F.);
#5503=ADVANCED_FACE('',(#759),#533,.F.);
#5504=ADVANCED_FACE('',(#760),#534,.F.);
#5505=ADVANCED_FACE('',(#761,#407),#5220,.T.);
#5506=ADVANCED_FACE('',(#762),#535,.T.);
#5507=ADVANCED_FACE('',(#763,#408),#536,.T.);
#5508=ADVANCED_FACE('',(#764,#409),#537,.F.);
#5509=ADVANCED_FACE('',(#765),#5221,.T.);
#5510=ADVANCED_FACE('',(#766),#5222,.T.);
#5511=ADVANCED_FACE('',(#767),#5223,.T.);
#5512=ADVANCED_FACE('',(#768,#410),#538,.T.);
#5513=ADVANCED_FACE('',(#769),#539,.F.);
#5514=ADVANCED_FACE('',(#770),#5224,.F.);
#5515=ADVANCED_FACE('',(#771),#5225,.T.);
#5516=ADVANCED_FACE('',(#772,#411),#540,.T.);
#5517=ADVANCED_FACE('',(#773,#412),#541,.F.);
#5518=ADVANCED_FACE('',(#774),#542,.T.);
#5519=ADVANCED_FACE('',(#775),#5226,.F.);
#5520=ADVANCED_FACE('',(#776),#543,.T.);
#5521=ADVANCED_FACE('',(#777,#413),#5227,.F.);
#5522=ADVANCED_FACE('',(#778,#414),#5228,.T.);
#5523=ADVANCED_FACE('',(#779,#415),#544,.T.);
#5524=ADVANCED_FACE('',(#780,#416),#545,.F.);
#5525=ADVANCED_FACE('',(#781),#546,.T.);
#5526=ADVANCED_FACE('',(#782),#5229,.F.);
#5527=ADVANCED_FACE('',(#783),#547,.T.);
#5528=ADVANCED_FACE('',(#784,#417),#5230,.F.);
#5529=ADVANCED_FACE('',(#785,#418),#5231,.T.);
#5530=ADVANCED_FACE('',(#786,#419),#548,.T.);
#5531=ADVANCED_FACE('',(#787,#420),#549,.F.);
#5532=ADVANCED_FACE('',(#788),#550,.F.);
#5533=ADVANCED_FACE('',(#789,#421),#551,.F.);
#5534=ADVANCED_FACE('',(#790),#552,.F.);
#5535=ADVANCED_FACE('',(#791,#422),#553,.T.);
#5536=ADVANCED_FACE('',(#792,#423,#424,#425),#5232,.F.);
#5537=ADVANCED_FACE('',(#793),#5233,.F.);
#5538=ADVANCED_FACE('',(#794),#5234,.F.);
#5539=ADVANCED_FACE('',(#795,#426,#427,#428),#5235,.T.);
#5540=ADVANCED_FACE('',(#796),#5236,.F.);
#5541=ADVANCED_FACE('',(#797),#5237,.F.);
#5542=ADVANCED_FACE('',(#798,#429),#554,.F.);
#5543=ADVANCED_FACE('',(#799,#430),#555,.T.);
#5544=ADVANCED_FACE('',(#800),#5238,.T.);
#5545=ADVANCED_FACE('',(#801,#431),#556,.F.);
#5546=ADVANCED_FACE('',(#802,#432),#557,.F.);
#5547=ADVANCED_FACE('',(#803),#5239,.T.);
#5548=ADVANCED_FACE('',(#804),#5240,.F.);
#5549=ADVANCED_FACE('',(#805),#5241,.T.);
#5550=ADVANCED_FACE('',(#806),#5242,.F.);
#5551=ADVANCED_FACE('',(#807),#5243,.T.);
#5552=ADVANCED_FACE('',(#808),#5244,.F.);
#5553=ADVANCED_FACE('',(#809),#5245,.T.);
#5554=ADVANCED_FACE('',(#810),#5246,.F.);
#5555=ADVANCED_FACE('',(#811),#5247,.T.);
#5556=ADVANCED_FACE('',(#812),#5248,.F.);
#5557=ADVANCED_FACE('',(#813),#5249,.T.);
#5558=ADVANCED_FACE('',(#814),#5250,.F.);
#5559=ADVANCED_FACE('',(#815),#5251,.T.);
#5560=ADVANCED_FACE('',(#816),#5252,.F.);
#5561=ADVANCED_FACE('',(#817),#5253,.T.);
#5562=ADVANCED_FACE('',(#818),#5254,.F.);
#5563=ADVANCED_FACE('',(#819),#5255,.T.);
#5564=ADVANCED_FACE('',(#820),#5256,.F.);
#5565=ADVANCED_FACE('',(#821),#5257,.T.);
#5566=ADVANCED_FACE('',(#822),#5258,.F.);
#5567=ADVANCED_FACE('',(#823),#5259,.T.);
#5568=ADVANCED_FACE('',(#824),#5260,.F.);
#5569=ADVANCED_FACE('',(#825),#5261,.T.);
#5570=ADVANCED_FACE('',(#826),#5262,.F.);
#5571=ADVANCED_FACE('',(#827),#5263,.T.);
#5572=ADVANCED_FACE('',(#828),#5264,.F.);
#5573=ADVANCED_FACE('',(#829),#5265,.T.);
#5574=ADVANCED_FACE('',(#830),#5266,.F.);
#5575=ADVANCED_FACE('',(#831),#5267,.T.);
#5576=ADVANCED_FACE('',(#832),#5268,.F.);
#5577=ADVANCED_FACE('',(#833),#5269,.T.);
#5578=ADVANCED_FACE('',(#834),#5270,.F.);
#5579=ADVANCED_FACE('',(#835),#5271,.T.);
#5580=ADVANCED_FACE('',(#836),#5272,.F.);
#5581=ADVANCED_FACE('',(#837),#5273,.T.);
#5582=ADVANCED_FACE('',(#838),#5274,.F.);
#5583=ADVANCED_FACE('',(#839),#5275,.T.);
#5584=ADVANCED_FACE('',(#840),#5276,.F.);
#5585=ADVANCED_FACE('',(#841),#5277,.T.);
#5586=ADVANCED_FACE('',(#842),#5278,.F.);
#5587=ADVANCED_FACE('',(#843),#5279,.T.);
#5588=ADVANCED_FACE('',(#844),#5280,.F.);
#5589=ADVANCED_FACE('',(#845),#5281,.T.);
#5590=ADVANCED_FACE('',(#846),#5282,.F.);
#5591=ADVANCED_FACE('',(#847),#5283,.T.);
#5592=ADVANCED_FACE('',(#848),#5284,.F.);
#5593=ADVANCED_FACE('',(#849),#5285,.T.);
#5594=ADVANCED_FACE('',(#850),#5286,.F.);
#5595=ADVANCED_FACE('',(#851),#5287,.T.);
#5596=ADVANCED_FACE('',(#852),#5288,.F.);
#5597=ADVANCED_FACE('',(#853),#5289,.T.);
#5598=ADVANCED_FACE('',(#854),#5290,.F.);
#5599=ADVANCED_FACE('',(#855),#5291,.T.);
#5600=ADVANCED_FACE('',(#856),#5292,.F.);
#5601=ADVANCED_FACE('',(#857),#5293,.T.);
#5602=ADVANCED_FACE('',(#858),#5294,.F.);
#5603=ADVANCED_FACE('',(#859),#5295,.T.);
#5604=ADVANCED_FACE('',(#860),#5296,.F.);
#5605=ADVANCED_FACE('',(#861),#5297,.T.);
#5606=ADVANCED_FACE('',(#862),#5298,.F.);
#5607=ADVANCED_FACE('',(#863),#5299,.T.);
#5608=ADVANCED_FACE('',(#864),#5300,.F.);
#5609=ADVANCED_FACE('',(#865),#5301,.T.);
#5610=ADVANCED_FACE('',(#866),#5302,.F.);
#5611=ADVANCED_FACE('',(#867),#5303,.T.);
#5612=ADVANCED_FACE('',(#868),#5304,.F.);
#5613=ADVANCED_FACE('',(#869),#5305,.T.);
#5614=ADVANCED_FACE('',(#870),#5306,.F.);
#5615=ADVANCED_FACE('',(#871),#5307,.T.);
#5616=ADVANCED_FACE('',(#872),#5308,.F.);
#5617=ADVANCED_FACE('',(#873),#5309,.T.);
#5618=ADVANCED_FACE('',(#874),#5310,.F.);
#5619=ADVANCED_FACE('',(#875),#5311,.T.);
#5620=ADVANCED_FACE('',(#876),#5312,.F.);
#5621=ADVANCED_FACE('',(#877),#5313,.T.);
#5622=ADVANCED_FACE('',(#878),#5314,.F.);
#5623=ADVANCED_FACE('',(#879),#5315,.T.);
#5624=ADVANCED_FACE('',(#880),#5316,.F.);
#5625=ADVANCED_FACE('',(#881),#5317,.T.);
#5626=ADVANCED_FACE('',(#882),#5318,.F.);
#5627=ADVANCED_FACE('',(#883),#5319,.T.);
#5628=ADVANCED_FACE('',(#884),#558,.T.);
#5629=ADVANCED_FACE('',(#885),#559,.T.);
#5630=ADVANCED_FACE('',(#886),#560,.T.);
#5631=ADVANCED_FACE('',(#887),#561,.T.);
#5632=ADVANCED_FACE('',(#888),#562,.T.);
#5633=ADVANCED_FACE('',(#889),#563,.F.);
#5634=ADVANCED_FACE('',(#890),#564,.T.);
#5635=ADVANCED_FACE('',(#891),#565,.T.);
#5636=ADVANCED_FACE('',(#892),#566,.T.);
#5637=ADVANCED_FACE('',(#893),#567,.F.);
#5638=ADVANCED_FACE('',(#894),#568,.F.);
#5639=ADVANCED_FACE('',(#895),#569,.F.);
#5640=ADVANCED_FACE('',(#896),#570,.F.);
#5641=ADVANCED_FACE('',(#897),#571,.F.);
#5642=ADVANCED_FACE('',(#898),#572,.F.);
#5643=ADVANCED_FACE('',(#899),#573,.F.);
#5644=ADVANCED_FACE('',(#900),#574,.F.);
#5645=ADVANCED_FACE('',(#901,#433),#575,.T.);
#5646=ADVANCED_FACE('',(#902),#235,.T.);
#5647=ADVANCED_FACE('',(#903),#5320,.T.);
#5648=ADVANCED_FACE('',(#904),#236,.T.);
#5649=ADVANCED_FACE('',(#905),#576,.T.);
#5650=CLOSED_SHELL('',(#5321,#5322,#5323,#5324,#5325,#5326,#5327,#5328,
#5329,#5330));
#5651=CLOSED_SHELL('',(#5331,#5332,#5333,#5334,#5335,#5336,#5337,#5338,
#5339,#5340,#5341,#5342,#5343,#5344,#5345,#5346,#5347,#5348,#5349,#5350,
#5351,#5352,#5353,#5354,#5355,#5356,#5357,#5358,#5359,#5360,#5361,#5362,
#5363,#5364,#5365,#5366,#5367,#5368,#5369,#5370,#5371,#5372));
#5652=CLOSED_SHELL('',(#5373,#5374,#5375,#5376));
#5653=CLOSED_SHELL('',(#5377,#5378,#5379,#5380,#5381,#5382,#5383,#5384,
#5385,#5386,#5387,#5388));
#5654=CLOSED_SHELL('',(#5389,#5390,#5391,#5392));
#5655=CLOSED_SHELL('',(#5393,#5394,#5395,#5396,#5397,#5398,#5399,#5400,
#5401,#5402));
#5656=CLOSED_SHELL('',(#5403,#5404,#5405,#5406,#5407,#5408));
#5657=CLOSED_SHELL('',(#5409,#5410,#5411,#5412,#5413,#5414));
#5658=CLOSED_SHELL('',(#5415,#5416,#5417,#5418,#5419,#5420,#5421,#5422));
#5659=CLOSED_SHELL('',(#5423,#5424,#5425,#5426,#5427,#5428,#5429,#5430));
#5660=CLOSED_SHELL('',(#5431));
#5661=CLOSED_SHELL('',(#5432));
#5662=CLOSED_SHELL('',(#5433));
#5663=CLOSED_SHELL('',(#5434));
#5664=CLOSED_SHELL('',(#5435));
#5665=CLOSED_SHELL('',(#5436));
#5666=CLOSED_SHELL('',(#5437));
#5667=CLOSED_SHELL('',(#5438));
#5668=CLOSED_SHELL('',(#5439,#5440,#5441,#5442,#5443,#5444,#5445,#5446,
#5447,#5448,#5449,#5450,#5451,#5452,#5453,#5454,#5455,#5456,#5457));
#5669=CLOSED_SHELL('',(#5458,#5459,#5460,#5461));
#5670=CLOSED_SHELL('',(#5462,#5463,#5464,#5465));
#5671=CLOSED_SHELL('',(#5466,#5467,#5468,#5469,#5470,#5471,#5472,#5473,
#5474));
#5672=CLOSED_SHELL('',(#5475,#5476,#5477,#5478,#5479,#5480,#5481,#5482));
#5673=CLOSED_SHELL('',(#5483,#5484,#5485,#5486,#5487,#5488,#5489,#5490,
#5491));
#5674=CLOSED_SHELL('',(#5492,#5493,#5494,#5495,#5496,#5497,#5498,#5499));
#5675=CLOSED_SHELL('',(#5500,#5501,#5502,#5503,#5504,#5505,#5506,#5507,
#5508,#5509,#5510,#5511,#5512,#5513));
#5676=CLOSED_SHELL('',(#5514,#5515,#5516,#5517));
#5677=CLOSED_SHELL('',(#5518,#5519,#5520,#5521,#5522,#5523,#5524));
#5678=CLOSED_SHELL('',(#5525,#5526,#5527,#5528,#5529,#5530,#5531));
#5679=CLOSED_SHELL('',(#5532,#5533,#5534,#5535,#5536,#5537,#5538,#5539,
#5540,#5541,#5542,#5543,#5544,#5545,#5546,#5547,#5548,#5549,#5550,#5551,
#5552,#5553,#5554,#5555,#5556,#5557,#5558,#5559,#5560,#5561,#5562,#5563,
#5564,#5565,#5566,#5567,#5568,#5569,#5570,#5571,#5572,#5573,#5574,#5575,
#5576,#5577,#5578,#5579,#5580,#5581,#5582,#5583,#5584,#5585,#5586,#5587,
#5588,#5589,#5590,#5591,#5592,#5593,#5594,#5595,#5596,#5597,#5598,#5599,
#5600,#5601,#5602,#5603,#5604,#5605,#5606,#5607,#5608,#5609,#5610,#5611,
#5612,#5613,#5614,#5615,#5616,#5617,#5618,#5619,#5620,#5621,#5622,#5623,
#5624,#5625,#5626,#5627));
#5680=CLOSED_SHELL('',(#5628,#5629,#5630,#5631,#5632,#5633,#5634,#5635,
#5636,#5637));
#5681=CLOSED_SHELL('',(#5638,#5639,#5640,#5641,#5642,#5643,#5644,#5645,
#5646,#5647,#5648,#5649));
#5682=DERIVED_UNIT_ELEMENT(#5726,1.);
#5683=DERIVED_UNIT_ELEMENT(#10965,-3.);
#5684=DERIVED_UNIT_ELEMENT(#5726,1.);
#5685=DERIVED_UNIT_ELEMENT(#10965,-3.);
#5686=DERIVED_UNIT_ELEMENT(#5726,1.);
#5687=DERIVED_UNIT_ELEMENT(#10965,-3.);
#5688=DERIVED_UNIT_ELEMENT(#5726,1.);
#5689=DERIVED_UNIT_ELEMENT(#10965,-3.);
#5690=DERIVED_UNIT_ELEMENT(#5726,1.);
#5691=DERIVED_UNIT_ELEMENT(#10965,-3.);
#5692=DERIVED_UNIT_ELEMENT(#5726,1.);
#5693=DERIVED_UNIT_ELEMENT(#10965,-3.);
#5694=DERIVED_UNIT_ELEMENT(#5726,1.);
#5695=DERIVED_UNIT_ELEMENT(#10965,-3.);
#5696=DERIVED_UNIT_ELEMENT(#5726,1.);
#5697=DERIVED_UNIT_ELEMENT(#10965,-3.);
#5698=DERIVED_UNIT_ELEMENT(#5726,1.);
#5699=DERIVED_UNIT_ELEMENT(#10965,-3.);
#5700=DERIVED_UNIT_ELEMENT(#5726,1.);
#5701=DERIVED_UNIT_ELEMENT(#10965,-3.);
#5702=DERIVED_UNIT_ELEMENT(#5726,1.);
#5703=DERIVED_UNIT_ELEMENT(#10965,-3.);
#5704=DERIVED_UNIT_ELEMENT(#5726,1.);
#5705=DERIVED_UNIT_ELEMENT(#10965,-3.);
#5706=DERIVED_UNIT_ELEMENT(#5726,1.);
#5707=DERIVED_UNIT_ELEMENT(#10965,-3.);
#5708=DERIVED_UNIT_ELEMENT(#5726,1.);
#5709=DERIVED_UNIT_ELEMENT(#10965,-3.);
#5710=DERIVED_UNIT_ELEMENT(#5726,1.);
#5711=DERIVED_UNIT_ELEMENT(#10965,-3.);
#5712=DERIVED_UNIT_ELEMENT(#5726,1.);
#5713=DERIVED_UNIT_ELEMENT(#10965,-3.);
#5714=DERIVED_UNIT_ELEMENT(#5726,1.);
#5715=DERIVED_UNIT_ELEMENT(#10965,-3.);
#5716=DERIVED_UNIT_ELEMENT(#5726,1.);
#5717=DERIVED_UNIT_ELEMENT(#10965,-3.);
#5718=DERIVED_UNIT_ELEMENT(#5726,1.);
#5719=DERIVED_UNIT_ELEMENT(#10965,-3.);
#5720=DERIVED_UNIT_ELEMENT(#5726,1.);
#5721=DERIVED_UNIT_ELEMENT(#10965,-3.);
#5722=DERIVED_UNIT_ELEMENT(#5726,1.);
#5723=DERIVED_UNIT_ELEMENT(#10965,-3.);
#5724=DERIVED_UNIT_ELEMENT(#5726,1.);
#5725=DERIVED_UNIT_ELEMENT(#10965,-3.);
#5726=(
MASS_UNIT()
NAMED_UNIT(*)
SI_UNIT(.KILO.,.GRAM.)
);
#5727=DERIVED_UNIT((#5682,#5683));
#5728=DERIVED_UNIT((#5684,#5685));
#5729=DERIVED_UNIT((#5686,#5687));
#5730=DERIVED_UNIT((#5688,#5689));
#5731=DERIVED_UNIT((#5690,#5691));
#5732=DERIVED_UNIT((#5692,#5693));
#5733=DERIVED_UNIT((#5694,#5695));
#5734=DERIVED_UNIT((#5696,#5697));
#5735=DERIVED_UNIT((#5698,#5699));
#5736=DERIVED_UNIT((#5700,#5701));
#5737=DERIVED_UNIT((#5702,#5703));
#5738=DERIVED_UNIT((#5704,#5705));
#5739=DERIVED_UNIT((#5706,#5707));
#5740=DERIVED_UNIT((#5708,#5709));
#5741=DERIVED_UNIT((#5710,#5711));
#5742=DERIVED_UNIT((#5712,#5713));
#5743=DERIVED_UNIT((#5714,#5715));
#5744=DERIVED_UNIT((#5716,#5717));
#5745=DERIVED_UNIT((#5718,#5719));
#5746=DERIVED_UNIT((#5720,#5721));
#5747=DERIVED_UNIT((#5722,#5723));
#5748=DERIVED_UNIT((#5724,#5725));
#5749=MEASURE_REPRESENTATION_ITEM('density measure',
POSITIVE_RATIO_MEASURE(7850.),#5727);
#5750=MEASURE_REPRESENTATION_ITEM('density measure',
POSITIVE_RATIO_MEASURE(7850.),#5728);
#5751=MEASURE_REPRESENTATION_ITEM('density measure',
POSITIVE_RATIO_MEASURE(7850.),#5729);
#5752=MEASURE_REPRESENTATION_ITEM('density measure',
POSITIVE_RATIO_MEASURE(7850.),#5730);
#5753=MEASURE_REPRESENTATION_ITEM('density measure',
POSITIVE_RATIO_MEASURE(7850.),#5731);
#5754=MEASURE_REPRESENTATION_ITEM('density measure',
POSITIVE_RATIO_MEASURE(7850.),#5732);
#5755=MEASURE_REPRESENTATION_ITEM('density measure',
POSITIVE_RATIO_MEASURE(7850.),#5733);
#5756=MEASURE_REPRESENTATION_ITEM('density measure',
POSITIVE_RATIO_MEASURE(7850.),#5734);
#5757=MEASURE_REPRESENTATION_ITEM('density measure',
POSITIVE_RATIO_MEASURE(7850.),#5735);
#5758=MEASURE_REPRESENTATION_ITEM('density measure',
POSITIVE_RATIO_MEASURE(7850.),#5736);
#5759=MEASURE_REPRESENTATION_ITEM('density measure',
POSITIVE_RATIO_MEASURE(7850.),#5737);
#5760=MEASURE_REPRESENTATION_ITEM('density measure',
POSITIVE_RATIO_MEASURE(7850.),#5738);
#5761=MEASURE_REPRESENTATION_ITEM('density measure',
POSITIVE_RATIO_MEASURE(7850.),#5739);
#5762=MEASURE_REPRESENTATION_ITEM('density measure',
POSITIVE_RATIO_MEASURE(7850.),#5740);
#5763=MEASURE_REPRESENTATION_ITEM('density measure',
POSITIVE_RATIO_MEASURE(7850.),#5741);
#5764=MEASURE_REPRESENTATION_ITEM('density measure',
POSITIVE_RATIO_MEASURE(7850.),#5742);
#5765=MEASURE_REPRESENTATION_ITEM('density measure',
POSITIVE_RATIO_MEASURE(7850.),#5743);
#5766=MEASURE_REPRESENTATION_ITEM('density measure',
POSITIVE_RATIO_MEASURE(7850.),#5744);
#5767=MEASURE_REPRESENTATION_ITEM('density measure',
POSITIVE_RATIO_MEASURE(7850.),#5745);
#5768=MEASURE_REPRESENTATION_ITEM('density measure',
POSITIVE_RATIO_MEASURE(7850.),#5746);
#5769=MEASURE_REPRESENTATION_ITEM('density measure',
POSITIVE_RATIO_MEASURE(7850.),#5747);
#5770=MEASURE_REPRESENTATION_ITEM('density measure',
POSITIVE_RATIO_MEASURE(7850.),#5748);
#5771=PROPERTY_DEFINITION_REPRESENTATION(#5881,#5815);
#5772=PROPERTY_DEFINITION_REPRESENTATION(#5882,#5816);
#5773=PROPERTY_DEFINITION_REPRESENTATION(#5883,#5817);
#5774=PROPERTY_DEFINITION_REPRESENTATION(#5884,#5818);
#5775=PROPERTY_DEFINITION_REPRESENTATION(#5885,#5819);
#5776=PROPERTY_DEFINITION_REPRESENTATION(#5886,#5820);
#5777=PROPERTY_DEFINITION_REPRESENTATION(#5887,#5821);
#5778=PROPERTY_DEFINITION_REPRESENTATION(#5888,#5822);
#5779=PROPERTY_DEFINITION_REPRESENTATION(#5889,#5823);
#5780=PROPERTY_DEFINITION_REPRESENTATION(#5890,#5824);
#5781=PROPERTY_DEFINITION_REPRESENTATION(#5891,#5825);
#5782=PROPERTY_DEFINITION_REPRESENTATION(#5892,#5826);
#5783=PROPERTY_DEFINITION_REPRESENTATION(#5893,#5827);
#5784=PROPERTY_DEFINITION_REPRESENTATION(#5894,#5828);
#5785=PROPERTY_DEFINITION_REPRESENTATION(#5895,#5829);
#5786=PROPERTY_DEFINITION_REPRESENTATION(#5896,#5830);
#5787=PROPERTY_DEFINITION_REPRESENTATION(#5897,#5831);
#5788=PROPERTY_DEFINITION_REPRESENTATION(#5898,#5832);
#5789=PROPERTY_DEFINITION_REPRESENTATION(#5899,#5833);
#5790=PROPERTY_DEFINITION_REPRESENTATION(#5900,#5834);
#5791=PROPERTY_DEFINITION_REPRESENTATION(#5901,#5835);
#5792=PROPERTY_DEFINITION_REPRESENTATION(#5902,#5836);
#5793=PROPERTY_DEFINITION_REPRESENTATION(#5903,#5837);
#5794=PROPERTY_DEFINITION_REPRESENTATION(#5904,#5838);
#5795=PROPERTY_DEFINITION_REPRESENTATION(#5905,#5839);
#5796=PROPERTY_DEFINITION_REPRESENTATION(#5906,#5840);
#5797=PROPERTY_DEFINITION_REPRESENTATION(#5907,#5841);
#5798=PROPERTY_DEFINITION_REPRESENTATION(#5908,#5842);
#5799=PROPERTY_DEFINITION_REPRESENTATION(#5909,#5843);
#5800=PROPERTY_DEFINITION_REPRESENTATION(#5910,#5844);
#5801=PROPERTY_DEFINITION_REPRESENTATION(#5911,#5845);
#5802=PROPERTY_DEFINITION_REPRESENTATION(#5912,#5846);
#5803=PROPERTY_DEFINITION_REPRESENTATION(#5913,#5847);
#5804=PROPERTY_DEFINITION_REPRESENTATION(#5914,#5848);
#5805=PROPERTY_DEFINITION_REPRESENTATION(#5915,#5849);
#5806=PROPERTY_DEFINITION_REPRESENTATION(#5916,#5850);
#5807=PROPERTY_DEFINITION_REPRESENTATION(#5917,#5851);
#5808=PROPERTY_DEFINITION_REPRESENTATION(#5918,#5852);
#5809=PROPERTY_DEFINITION_REPRESENTATION(#5919,#5853);
#5810=PROPERTY_DEFINITION_REPRESENTATION(#5920,#5854);
#5811=PROPERTY_DEFINITION_REPRESENTATION(#5921,#5855);
#5812=PROPERTY_DEFINITION_REPRESENTATION(#5922,#5856);
#5813=PROPERTY_DEFINITION_REPRESENTATION(#5923,#5857);
#5814=PROPERTY_DEFINITION_REPRESENTATION(#5924,#5858);
#5815=REPRESENTATION('material name',(#5859),#10939);
#5816=REPRESENTATION('density',(#5749),#10939);
#5817=REPRESENTATION('material name',(#5860),#10940);
#5818=REPRESENTATION('density',(#5750),#10940);
#5819=REPRESENTATION('material name',(#5861),#10941);
#5820=REPRESENTATION('density',(#5751),#10941);
#5821=REPRESENTATION('material name',(#5862),#10942);
#5822=REPRESENTATION('density',(#5752),#10942);
#5823=REPRESENTATION('material name',(#5863),#10943);
#5824=REPRESENTATION('density',(#5753),#10943);
#5825=REPRESENTATION('material name',(#5864),#10944);
#5826=REPRESENTATION('density',(#5754),#10944);
#5827=REPRESENTATION('material name',(#5865),#10945);
#5828=REPRESENTATION('density',(#5755),#10945);
#5829=REPRESENTATION('material name',(#5866),#10946);
#5830=REPRESENTATION('density',(#5756),#10946);
#5831=REPRESENTATION('material name',(#5867),#10948);
#5832=REPRESENTATION('density',(#5757),#10948);
#5833=REPRESENTATION('material name',(#5868),#10949);
#5834=REPRESENTATION('density',(#5758),#10949);
#5835=REPRESENTATION('material name',(#5869),#10950);
#5836=REPRESENTATION('density',(#5759),#10950);
#5837=REPRESENTATION('material name',(#5870),#10951);
#5838=REPRESENTATION('density',(#5760),#10951);
#5839=REPRESENTATION('material name',(#5871),#10952);
#5840=REPRESENTATION('density',(#5761),#10952);
#5841=REPRESENTATION('material name',(#5872),#10953);
#5842=REPRESENTATION('density',(#5762),#10953);
#5843=REPRESENTATION('material name',(#5873),#10954);
#5844=REPRESENTATION('density',(#5763),#10954);
#5845=REPRESENTATION('material name',(#5874),#10956);
#5846=REPRESENTATION('density',(#5764),#10956);
#5847=REPRESENTATION('material name',(#5875),#10957);
#5848=REPRESENTATION('density',(#5765),#10957);
#5849=REPRESENTATION('material name',(#5876),#10958);
#5850=REPRESENTATION('density',(#5766),#10958);
#5851=REPRESENTATION('material name',(#5877),#10959);
#5852=REPRESENTATION('density',(#5767),#10959);
#5853=REPRESENTATION('material name',(#5878),#10960);
#5854=REPRESENTATION('density',(#5768),#10960);
#5855=REPRESENTATION('material name',(#5879),#10961);
#5856=REPRESENTATION('density',(#5769),#10961);
#5857=REPRESENTATION('material name',(#5880),#10962);
#5858=REPRESENTATION('density',(#5770),#10962);
#5859=DESCRIPTIVE_REPRESENTATION_ITEM('Steel','Steel');
#5860=DESCRIPTIVE_REPRESENTATION_ITEM('Steel','Steel');
#5861=DESCRIPTIVE_REPRESENTATION_ITEM('Steel','Steel');
#5862=DESCRIPTIVE_REPRESENTATION_ITEM('Steel','Steel');
#5863=DESCRIPTIVE_REPRESENTATION_ITEM('Steel','Steel');
#5864=DESCRIPTIVE_REPRESENTATION_ITEM('Steel','Steel');
#5865=DESCRIPTIVE_REPRESENTATION_ITEM('Steel','Steel');
#5866=DESCRIPTIVE_REPRESENTATION_ITEM('Steel','Steel');
#5867=DESCRIPTIVE_REPRESENTATION_ITEM('Steel','Steel');
#5868=DESCRIPTIVE_REPRESENTATION_ITEM('Steel','Steel');
#5869=DESCRIPTIVE_REPRESENTATION_ITEM('Steel','Steel');
#5870=DESCRIPTIVE_REPRESENTATION_ITEM('Steel','Steel');
#5871=DESCRIPTIVE_REPRESENTATION_ITEM('Steel','Steel');
#5872=DESCRIPTIVE_REPRESENTATION_ITEM('Steel','Steel');
#5873=DESCRIPTIVE_REPRESENTATION_ITEM('Steel','Steel');
#5874=DESCRIPTIVE_REPRESENTATION_ITEM('Steel','Steel');
#5875=DESCRIPTIVE_REPRESENTATION_ITEM('Steel','Steel');
#5876=DESCRIPTIVE_REPRESENTATION_ITEM('Steel','Steel');
#5877=DESCRIPTIVE_REPRESENTATION_ITEM('Steel','Steel');
#5878=DESCRIPTIVE_REPRESENTATION_ITEM('Steel','Steel');
#5879=DESCRIPTIVE_REPRESENTATION_ITEM('Steel','Steel');
#5880=DESCRIPTIVE_REPRESENTATION_ITEM('Steel','Steel');
#5881=PROPERTY_DEFINITION('material property','material name',#11086);
#5882=PROPERTY_DEFINITION('material property','density of part',#11086);
#5883=PROPERTY_DEFINITION('material property','material name',#11087);
#5884=PROPERTY_DEFINITION('material property','density of part',#11087);
#5885=PROPERTY_DEFINITION('material property','material name',#11088);
#5886=PROPERTY_DEFINITION('material property','density of part',#11088);
#5887=PROPERTY_DEFINITION('material property','material name',#11089);
#5888=PROPERTY_DEFINITION('material property','density of part',#11089);
#5889=PROPERTY_DEFINITION('material property','material name',#11090);
#5890=PROPERTY_DEFINITION('material property','density of part',#11090);
#5891=PROPERTY_DEFINITION('material property','material name',#11091);
#5892=PROPERTY_DEFINITION('material property','density of part',#11091);
#5893=PROPERTY_DEFINITION('material property','material name',#11092);
#5894=PROPERTY_DEFINITION('material property','density of part',#11092);
#5895=PROPERTY_DEFINITION('material property','material name',#11093);
#5896=PROPERTY_DEFINITION('material property','density of part',#11093);
#5897=PROPERTY_DEFINITION('material property','material name',#11095);
#5898=PROPERTY_DEFINITION('material property','density of part',#11095);
#5899=PROPERTY_DEFINITION('material property','material name',#11096);
#5900=PROPERTY_DEFINITION('material property','density of part',#11096);
#5901=PROPERTY_DEFINITION('material property','material name',#11097);
#5902=PROPERTY_DEFINITION('material property','density of part',#11097);
#5903=PROPERTY_DEFINITION('material property','material name',#11098);
#5904=PROPERTY_DEFINITION('material property','density of part',#11098);
#5905=PROPERTY_DEFINITION('material property','material name',#11099);
#5906=PROPERTY_DEFINITION('material property','density of part',#11099);
#5907=PROPERTY_DEFINITION('material property','material name',#11100);
#5908=PROPERTY_DEFINITION('material property','density of part',#11100);
#5909=PROPERTY_DEFINITION('material property','material name',#11101);
#5910=PROPERTY_DEFINITION('material property','density of part',#11101);
#5911=PROPERTY_DEFINITION('material property','material name',#11103);
#5912=PROPERTY_DEFINITION('material property','density of part',#11103);
#5913=PROPERTY_DEFINITION('material property','material name',#11104);
#5914=PROPERTY_DEFINITION('material property','density of part',#11104);
#5915=PROPERTY_DEFINITION('material property','material name',#11105);
#5916=PROPERTY_DEFINITION('material property','density of part',#11105);
#5917=PROPERTY_DEFINITION('material property','material name',#11106);
#5918=PROPERTY_DEFINITION('material property','density of part',#11106);
#5919=PROPERTY_DEFINITION('material property','material name',#11107);
#5920=PROPERTY_DEFINITION('material property','density of part',#11107);
#5921=PROPERTY_DEFINITION('material property','material name',#11108);
#5922=PROPERTY_DEFINITION('material property','density of part',#11108);
#5923=PROPERTY_DEFINITION('material property','material name',#11109);
#5924=PROPERTY_DEFINITION('material property','density of part',#11109);
#5925=AXIS2_PLACEMENT_3D('',#8556,#6688,#6689);
#5926=AXIS2_PLACEMENT_3D('',#8557,#6690,#6691);
#5927=AXIS2_PLACEMENT_3D('',#8558,#6692,#6693);
#5928=AXIS2_PLACEMENT_3D('',#8559,#6694,#6695);
#5929=AXIS2_PLACEMENT_3D('',#8561,#6696,#6697);
#5930=AXIS2_PLACEMENT_3D('',#8564,#6699,#6700);
#5931=AXIS2_PLACEMENT_3D('',#8565,#6701,#6702);
#5932=AXIS2_PLACEMENT_3D('',#8567,#6703,#6704);
#5933=AXIS2_PLACEMENT_3D('',#8570,#6706,#6707);
#5934=AXIS2_PLACEMENT_3D('',#8571,#6708,#6709);
#5935=AXIS2_PLACEMENT_3D('',#8573,#6710,#6711);
#5936=AXIS2_PLACEMENT_3D('',#8576,#6713,#6714);
#5937=AXIS2_PLACEMENT_3D('',#8577,#6715,#6716);
#5938=AXIS2_PLACEMENT_3D('',#8579,#6717,#6718);
#5939=AXIS2_PLACEMENT_3D('',#8582,#6720,#6721);
#5940=AXIS2_PLACEMENT_3D('',#8583,#6722,#6723);
#5941=AXIS2_PLACEMENT_3D('',#8592,#6728,#6729);
#5942=AXIS2_PLACEMENT_3D('',#8598,#6733,#6734);
#5943=AXIS2_PLACEMENT_3D('',#8604,#6738,#6739);
#5944=AXIS2_PLACEMENT_3D('',#8607,#6742,#6743);
#5945=AXIS2_PLACEMENT_3D('',#8608,#6744,#6745);
#5946=AXIS2_PLACEMENT_3D('',#8609,#6746,#6747);
#5947=AXIS2_PLACEMENT_3D('',#8610,#6748,#6749);
#5948=AXIS2_PLACEMENT_3D('',#8612,#6750,#6751);
#5949=AXIS2_PLACEMENT_3D('',#8615,#6753,#6754);
#5950=AXIS2_PLACEMENT_3D('',#8616,#6755,#6756);
#5951=AXIS2_PLACEMENT_3D('',#8617,#6757,#6758);
#5952=AXIS2_PLACEMENT_3D('',#8619,#6759,#6760);
#5953=AXIS2_PLACEMENT_3D('',#8622,#6762,#6763);
#5954=AXIS2_PLACEMENT_3D('',#8623,#6764,#6765);
#5955=AXIS2_PLACEMENT_3D('',#8624,#6766,#6767);
#5956=AXIS2_PLACEMENT_3D('',#8626,#6768,#6769);
#5957=AXIS2_PLACEMENT_3D('',#8629,#6771,#6772);
#5958=AXIS2_PLACEMENT_3D('',#8630,#6773,#6774);
#5959=AXIS2_PLACEMENT_3D('',#8631,#6775,#6776);
#5960=AXIS2_PLACEMENT_3D('',#8633,#6777,#6778);
#5961=AXIS2_PLACEMENT_3D('',#8636,#6780,#6781);
#5962=AXIS2_PLACEMENT_3D('',#8637,#6782,#6783);
#5963=AXIS2_PLACEMENT_3D('',#8638,#6784,#6785);
#5964=AXIS2_PLACEMENT_3D('',#8640,#6786,#6787);
#5965=AXIS2_PLACEMENT_3D('',#8643,#6789,#6790);
#5966=AXIS2_PLACEMENT_3D('',#8644,#6791,#6792);
#5967=AXIS2_PLACEMENT_3D('',#8645,#6793,#6794);
#5968=AXIS2_PLACEMENT_3D('',#8647,#6795,#6796);
#5969=AXIS2_PLACEMENT_3D('',#8650,#6798,#6799);
#5970=AXIS2_PLACEMENT_3D('',#8651,#6800,#6801);
#5971=AXIS2_PLACEMENT_3D('',#8652,#6802,#6803);
#5972=AXIS2_PLACEMENT_3D('',#8654,#6804,#6805);
#5973=AXIS2_PLACEMENT_3D('',#8657,#6807,#6808);
#5974=AXIS2_PLACEMENT_3D('',#8658,#6809,#6810);
#5975=AXIS2_PLACEMENT_3D('',#8659,#6811,#6812);
#5976=AXIS2_PLACEMENT_3D('',#8661,#6813,#6814);
#5977=AXIS2_PLACEMENT_3D('',#8664,#6816,#6817);
#5978=AXIS2_PLACEMENT_3D('',#8665,#6818,#6819);
#5979=AXIS2_PLACEMENT_3D('',#8666,#6820,#6821);
#5980=AXIS2_PLACEMENT_3D('',#8668,#6822,#6823);
#5981=AXIS2_PLACEMENT_3D('',#8671,#6825,#6826);
#5982=AXIS2_PLACEMENT_3D('',#8672,#6827,#6828);
#5983=AXIS2_PLACEMENT_3D('',#8674,#6829,#6830);
#5984=AXIS2_PLACEMENT_3D('',#8677,#6832,#6833);
#5985=AXIS2_PLACEMENT_3D('',#8678,#6834,#6835);
#5986=AXIS2_PLACEMENT_3D('',#8680,#6836,#6837);
#5987=AXIS2_PLACEMENT_3D('',#8683,#6839,#6840);
#5988=AXIS2_PLACEMENT_3D('',#8684,#6841,#6842);
#5989=AXIS2_PLACEMENT_3D('',#8686,#6843,#6844);
#5990=AXIS2_PLACEMENT_3D('',#8689,#6846,#6847);
#5991=AXIS2_PLACEMENT_3D('',#8690,#6848,#6849);
#5992=AXIS2_PLACEMENT_3D('',#8693,#6850,#6851);
#5993=AXIS2_PLACEMENT_3D('',#8699,#6855,#6856);
#5994=AXIS2_PLACEMENT_3D('',#8701,#6857,#6858);
#5995=AXIS2_PLACEMENT_3D('',#8707,#6862,#6863);
#5996=AXIS2_PLACEMENT_3D('',#8710,#6864,#6865);
#5997=AXIS2_PLACEMENT_3D('',#8716,#6869,#6870);
#5998=AXIS2_PLACEMENT_3D('',#8718,#6871,#6872);
#5999=AXIS2_PLACEMENT_3D('',#8724,#6876,#6877);
#6000=AXIS2_PLACEMENT_3D('',#8727,#6880,#6881);
#6001=AXIS2_PLACEMENT_3D('',#8730,#6884,#6885);
#6002=AXIS2_PLACEMENT_3D('',#8732,#6887,#6888);
#6003=AXIS2_PLACEMENT_3D('',#8734,#6890,#6891);
#6004=AXIS2_PLACEMENT_3D('',#8735,#6892,#6893);
#6005=AXIS2_PLACEMENT_3D('',#8738,#6894,#6895);
#6006=AXIS2_PLACEMENT_3D('',#8744,#6899,#6900);
#6007=AXIS2_PLACEMENT_3D('',#8746,#6901,#6902);
#6008=AXIS2_PLACEMENT_3D('',#8752,#6906,#6907);
#6009=AXIS2_PLACEMENT_3D('',#8755,#6908,#6909);
#6010=AXIS2_PLACEMENT_3D('',#8761,#6913,#6914);
#6011=AXIS2_PLACEMENT_3D('',#8763,#6915,#6916);
#6012=AXIS2_PLACEMENT_3D('',#8769,#6920,#6921);
#6013=AXIS2_PLACEMENT_3D('',#8772,#6924,#6925);
#6014=AXIS2_PLACEMENT_3D('',#8775,#6928,#6929);
#6015=AXIS2_PLACEMENT_3D('',#8777,#6931,#6932);
#6016=AXIS2_PLACEMENT_3D('',#8779,#6934,#6935);
#6017=AXIS2_PLACEMENT_3D('',#8780,#6936,#6937);
#6018=AXIS2_PLACEMENT_3D('',#8782,#6938,#6939);
#6019=AXIS2_PLACEMENT_3D('',#8785,#6941,#6942);
#6020=AXIS2_PLACEMENT_3D('',#8786,#6943,#6944);
#6021=AXIS2_PLACEMENT_3D('',#8788,#6945,#6946);
#6022=AXIS2_PLACEMENT_3D('',#8791,#6948,#6949);
#6023=AXIS2_PLACEMENT_3D('',#8792,#6950,#6951);
#6024=AXIS2_PLACEMENT_3D('',#8793,#6952,#6953);
#6025=AXIS2_PLACEMENT_3D('',#8794,#6954,#6955);
#6026=AXIS2_PLACEMENT_3D('',#8795,#6956,#6957);
#6027=AXIS2_PLACEMENT_3D('',#8797,#6958,#6959);
#6028=AXIS2_PLACEMENT_3D('',#8800,#6961,#6962);
#6029=AXIS2_PLACEMENT_3D('',#8801,#6963,#6964);
#6030=AXIS2_PLACEMENT_3D('',#8803,#6965,#6966);
#6031=AXIS2_PLACEMENT_3D('',#8806,#6968,#6969);
#6032=AXIS2_PLACEMENT_3D('',#8807,#6970,#6971);
#6033=AXIS2_PLACEMENT_3D('',#8808,#6972,#6973);
#6034=AXIS2_PLACEMENT_3D('',#8809,#6974,#6975);
#6035=AXIS2_PLACEMENT_3D('',#8810,#6976,#6977);
#6036=AXIS2_PLACEMENT_3D('',#8812,#6978,#6979);
#6037=AXIS2_PLACEMENT_3D('',#8815,#6981,#6982);
#6038=AXIS2_PLACEMENT_3D('',#8816,#6983,#6984);
#6039=AXIS2_PLACEMENT_3D('',#8818,#6985,#6986);
#6040=AXIS2_PLACEMENT_3D('',#8821,#6988,#6989);
#6041=AXIS2_PLACEMENT_3D('',#8822,#6990,#6991);
#6042=AXIS2_PLACEMENT_3D('',#8824,#6992,#6993);
#6043=AXIS2_PLACEMENT_3D('',#8827,#6995,#6996);
#6044=AXIS2_PLACEMENT_3D('',#8828,#6997,#6998);
#6045=AXIS2_PLACEMENT_3D('',#8830,#6999,#7000);
#6046=AXIS2_PLACEMENT_3D('',#8833,#7002,#7003);
#6047=AXIS2_PLACEMENT_3D('',#8834,#7004,#7005);
#6048=AXIS2_PLACEMENT_3D('',#8836,#7006,#7007);
#6049=AXIS2_PLACEMENT_3D('',#8839,#7009,#7010);
#6050=AXIS2_PLACEMENT_3D('',#8840,#7011,#7012);
#6051=AXIS2_PLACEMENT_3D('',#8842,#7013,#7014);
#6052=AXIS2_PLACEMENT_3D('',#8843,#7015,#7016);
#6053=AXIS2_PLACEMENT_3D('',#8845,#7017,#7018);
#6054=AXIS2_PLACEMENT_3D('',#8848,#7020,#7021);
#6055=AXIS2_PLACEMENT_3D('',#8849,#7022,#7023);
#6056=AXIS2_PLACEMENT_3D('',#8851,#7024,#7025);
#6057=AXIS2_PLACEMENT_3D('',#8852,#7026,#7027);
#6058=AXIS2_PLACEMENT_3D('',#8854,#7029,#7030);
#6059=AXIS2_PLACEMENT_3D('',#8856,#7031,#7032);
#6060=AXIS2_PLACEMENT_3D('',#8859,#7034,#7035);
#6061=AXIS2_PLACEMENT_3D('',#8860,#7036,#7037);
#6062=AXIS2_PLACEMENT_3D('',#8861,#7038,#7039);
#6063=AXIS2_PLACEMENT_3D('',#8862,#7040,#7041);
#6064=AXIS2_PLACEMENT_3D('',#8863,#7042,#7043);
#6065=AXIS2_PLACEMENT_3D('',#8865,#7044,#7045);
#6066=AXIS2_PLACEMENT_3D('',#8868,#7047,#7048);
#6067=AXIS2_PLACEMENT_3D('',#8869,#7049,#7050);
#6068=AXIS2_PLACEMENT_3D('',#8871,#7051,#7052);
#6069=AXIS2_PLACEMENT_3D('',#8874,#7054,#7055);
#6070=AXIS2_PLACEMENT_3D('',#8875,#7056,#7057);
#6071=AXIS2_PLACEMENT_3D('',#8876,#7058,#7059);
#6072=AXIS2_PLACEMENT_3D('',#8877,#7060,#7061);
#6073=AXIS2_PLACEMENT_3D('',#8878,#7062,#7063);
#6074=AXIS2_PLACEMENT_3D('',#8880,#7064,#7065);
#6075=AXIS2_PLACEMENT_3D('',#8883,#7067,#7068);
#6076=AXIS2_PLACEMENT_3D('',#8884,#7069,#7070);
#6077=AXIS2_PLACEMENT_3D('',#8886,#7071,#7072);
#6078=AXIS2_PLACEMENT_3D('',#8889,#7074,#7075);
#6079=AXIS2_PLACEMENT_3D('',#8890,#7076,#7077);
#6080=AXIS2_PLACEMENT_3D('',#8892,#7078,#7079);
#6081=AXIS2_PLACEMENT_3D('',#8895,#7081,#7082);
#6082=AXIS2_PLACEMENT_3D('',#8896,#7083,#7084);
#6083=AXIS2_PLACEMENT_3D('',#8898,#7085,#7086);
#6084=AXIS2_PLACEMENT_3D('',#8901,#7088,#7089);
#6085=AXIS2_PLACEMENT_3D('',#8902,#7090,#7091);
#6086=AXIS2_PLACEMENT_3D('',#8904,#7092,#7093);
#6087=AXIS2_PLACEMENT_3D('',#8907,#7095,#7096);
#6088=AXIS2_PLACEMENT_3D('',#8908,#7097,#7098);
#6089=AXIS2_PLACEMENT_3D('',#8910,#7099,#7100);
#6090=AXIS2_PLACEMENT_3D('',#8911,#7101,#7102);
#6091=AXIS2_PLACEMENT_3D('',#8913,#7103,#7104);
#6092=AXIS2_PLACEMENT_3D('',#8915,#7106,#7107);
#6093=AXIS2_PLACEMENT_3D('',#8917,#7108,#7109);
#6094=AXIS2_PLACEMENT_3D('',#8920,#7111,#7112);
#6095=AXIS2_PLACEMENT_3D('',#8921,#7113,#7114);
#6096=AXIS2_PLACEMENT_3D('',#8922,#7115,#7116);
#6097=AXIS2_PLACEMENT_3D('',#8923,#7117,#7118);
#6098=AXIS2_PLACEMENT_3D('',#8924,#7119,#7120);
#6099=AXIS2_PLACEMENT_3D('',#8933,#7125,#7126);
#6100=AXIS2_PLACEMENT_3D('',#8939,#7130,#7131);
#6101=AXIS2_PLACEMENT_3D('',#8945,#7135,#7136);
#6102=AXIS2_PLACEMENT_3D('',#8948,#7139,#7140);
#6103=AXIS2_PLACEMENT_3D('',#8949,#7141,#7142);
#6104=AXIS2_PLACEMENT_3D('',#8950,#7143,#7144);
#6105=AXIS2_PLACEMENT_3D('',#8951,#7145,#7146);
#6106=AXIS2_PLACEMENT_3D('',#8960,#7151,#7152);
#6107=AXIS2_PLACEMENT_3D('',#8966,#7156,#7157);
#6108=AXIS2_PLACEMENT_3D('',#8972,#7161,#7162);
#6109=AXIS2_PLACEMENT_3D('',#8975,#7165,#7166);
#6110=AXIS2_PLACEMENT_3D('',#8976,#7167,#7168);
#6111=AXIS2_PLACEMENT_3D('',#8977,#7169,#7170);
#6112=AXIS2_PLACEMENT_3D('',#8978,#7171,#7172);
#6113=AXIS2_PLACEMENT_3D('',#8979,#7173,#7174);
#6114=AXIS2_PLACEMENT_3D('',#8982,#7175,#7176);
#6115=AXIS2_PLACEMENT_3D('',#8983,#7177,#7178);
#6116=AXIS2_PLACEMENT_3D('',#8985,#7179,#7180);
#6117=AXIS2_PLACEMENT_3D('',#8987,#7181,#7182);
#6118=AXIS2_PLACEMENT_3D('',#8988,#7183,#7184);
#6119=AXIS2_PLACEMENT_3D('',#8989,#7185,#7186);
#6120=AXIS2_PLACEMENT_3D('',#8992,#7188,#7189);
#6121=AXIS2_PLACEMENT_3D('',#8993,#7190,#7191);
#6122=AXIS2_PLACEMENT_3D('',#8995,#7192,#7193);
#6123=AXIS2_PLACEMENT_3D('',#8998,#7195,#7196);
#6124=AXIS2_PLACEMENT_3D('',#8999,#7197,#7198);
#6125=AXIS2_PLACEMENT_3D('',#9002,#7200,#7201);
#6126=AXIS2_PLACEMENT_3D('',#9003,#7202,#7203);
#6127=AXIS2_PLACEMENT_3D('',#9004,#7204,#7205);
#6128=AXIS2_PLACEMENT_3D('',#9006,#7206,#7207);
#6129=AXIS2_PLACEMENT_3D('',#9008,#7209,#7210);
#6130=AXIS2_PLACEMENT_3D('',#9010,#7211,#7212);
#6131=AXIS2_PLACEMENT_3D('',#9011,#7213,#7214);
#6132=AXIS2_PLACEMENT_3D('',#9013,#7216,#7217);
#6133=AXIS2_PLACEMENT_3D('',#9014,#7218,#7219);
#6134=AXIS2_PLACEMENT_3D('',#9017,#7220,#7221);
#6135=AXIS2_PLACEMENT_3D('',#9018,#7222,#7223);
#6136=AXIS2_PLACEMENT_3D('',#9020,#7224,#7225);
#6137=AXIS2_PLACEMENT_3D('',#9022,#7226,#7227);
#6138=AXIS2_PLACEMENT_3D('',#9023,#7228,#7229);
#6139=AXIS2_PLACEMENT_3D('',#9024,#7230,#7231);
#6140=AXIS2_PLACEMENT_3D('',#9026,#7232,#7233);
#6141=AXIS2_PLACEMENT_3D('',#9028,#7235,#7236);
#6142=AXIS2_PLACEMENT_3D('',#9030,#7237,#7238);
#6143=AXIS2_PLACEMENT_3D('',#9032,#7239,#7240);
#6144=AXIS2_PLACEMENT_3D('',#9033,#7241,#7242);
#6145=AXIS2_PLACEMENT_3D('',#9035,#7243,#7244);
#6146=AXIS2_PLACEMENT_3D('',#9037,#7246,#7247);
#6147=AXIS2_PLACEMENT_3D('',#9039,#7248,#7249);
#6148=AXIS2_PLACEMENT_3D('',#9041,#7251,#7252);
#6149=AXIS2_PLACEMENT_3D('',#9043,#7253,#7254);
#6150=AXIS2_PLACEMENT_3D('',#9045,#7256,#7257);
#6151=AXIS2_PLACEMENT_3D('',#9046,#7258,#7259);
#6152=AXIS2_PLACEMENT_3D('',#9048,#7261,#7262);
#6153=AXIS2_PLACEMENT_3D('',#9049,#7263,#7264);
#6154=AXIS2_PLACEMENT_3D('',#9052,#7265,#7266);
#6155=AXIS2_PLACEMENT_3D('',#9053,#7267,#7268);
#6156=AXIS2_PLACEMENT_3D('',#9056,#7269,#7270);
#6157=AXIS2_PLACEMENT_3D('',#9057,#7271,#7272);
#6158=AXIS2_PLACEMENT_3D('',#9060,#7273,#7274);
#6159=AXIS2_PLACEMENT_3D('',#9061,#7275,#7276);
#6160=AXIS2_PLACEMENT_3D('',#9064,#7277,#7278);
#6161=AXIS2_PLACEMENT_3D('',#9065,#7279,#7280);
#6162=AXIS2_PLACEMENT_3D('',#9068,#7281,#7282);
#6163=AXIS2_PLACEMENT_3D('',#9069,#7283,#7284);
#6164=AXIS2_PLACEMENT_3D('',#9072,#7285,#7286);
#6165=AXIS2_PLACEMENT_3D('',#9073,#7287,#7288);
#6166=AXIS2_PLACEMENT_3D('',#9076,#7289,#7290);
#6167=AXIS2_PLACEMENT_3D('',#9077,#7291,#7292);
#6168=AXIS2_PLACEMENT_3D('',#9080,#7293,#7294);
#6169=AXIS2_PLACEMENT_3D('',#9081,#7295,#7296);
#6170=AXIS2_PLACEMENT_3D('',#9082,#7297,#7298);
#6171=AXIS2_PLACEMENT_3D('',#9108,#7299,#7300);
#6172=AXIS2_PLACEMENT_3D('',#9132,#7301,#7302);
#6173=AXIS2_PLACEMENT_3D('',#9133,#7303,#7304);
#6174=AXIS2_PLACEMENT_3D('',#9135,#7305,#7306);
#6175=AXIS2_PLACEMENT_3D('',#9160,#7307,#7308);
#6176=AXIS2_PLACEMENT_3D('',#9185,#7309,#7310);
#6177=AXIS2_PLACEMENT_3D('',#9201,#7312,#7313);
#6178=AXIS2_PLACEMENT_3D('',#9216,#7314,#7315);
#6179=AXIS2_PLACEMENT_3D('',#9241,#7316,#7317);
#6180=AXIS2_PLACEMENT_3D('',#9266,#7318,#7319);
#6181=AXIS2_PLACEMENT_3D('',#9291,#7320,#7321);
#6182=AXIS2_PLACEMENT_3D('',#9315,#7322,#7323);
#6183=AXIS2_PLACEMENT_3D('',#9316,#7324,#7325);
#6184=AXIS2_PLACEMENT_3D('',#9318,#7326,#7327);
#6185=AXIS2_PLACEMENT_3D('',#9319,#7328,#7329);
#6186=AXIS2_PLACEMENT_3D('',#9320,#7330,#7331);
#6187=AXIS2_PLACEMENT_3D('',#9344,#7332,#7333);
#6188=AXIS2_PLACEMENT_3D('',#9345,#7334,#7335);
#6189=AXIS2_PLACEMENT_3D('',#9347,#7336,#7337);
#6190=AXIS2_PLACEMENT_3D('',#9348,#7338,#7339);
#6191=AXIS2_PLACEMENT_3D('',#9349,#7340,#7341);
#6192=AXIS2_PLACEMENT_3D('',#9373,#7342,#7343);
#6193=AXIS2_PLACEMENT_3D('',#9374,#7344,#7345);
#6194=AXIS2_PLACEMENT_3D('',#9376,#7346,#7347);
#6195=AXIS2_PLACEMENT_3D('',#9377,#7348,#7349);
#6196=AXIS2_PLACEMENT_3D('',#9378,#7350,#7351);
#6197=AXIS2_PLACEMENT_3D('',#9393,#7352,#7353);
#6198=AXIS2_PLACEMENT_3D('',#9406,#7354,#7355);
#6199=AXIS2_PLACEMENT_3D('',#9408,#7356,#7357);
#6200=AXIS2_PLACEMENT_3D('',#9409,#7358,#7359);
#6201=AXIS2_PLACEMENT_3D('',#9410,#7360,#7361);
#6202=AXIS2_PLACEMENT_3D('',#9434,#7362,#7363);
#6203=AXIS2_PLACEMENT_3D('',#9435,#7364,#7365);
#6204=AXIS2_PLACEMENT_3D('',#9437,#7366,#7367);
#6205=AXIS2_PLACEMENT_3D('',#9438,#7368,#7369);
#6206=AXIS2_PLACEMENT_3D('',#9439,#7370,#7371);
#6207=AXIS2_PLACEMENT_3D('',#9463,#7372,#7373);
#6208=AXIS2_PLACEMENT_3D('',#9464,#7374,#7375);
#6209=AXIS2_PLACEMENT_3D('',#9466,#7376,#7377);
#6210=AXIS2_PLACEMENT_3D('',#9467,#7378,#7379);
#6211=AXIS2_PLACEMENT_3D('',#9468,#7380,#7381);
#6212=AXIS2_PLACEMENT_3D('',#9492,#7382,#7383);
#6213=AXIS2_PLACEMENT_3D('',#9493,#7384,#7385);
#6214=AXIS2_PLACEMENT_3D('',#9495,#7386,#7387);
#6215=AXIS2_PLACEMENT_3D('',#9498,#7389,#7390);
#6216=AXIS2_PLACEMENT_3D('',#9522,#7391,#7392);
#6217=AXIS2_PLACEMENT_3D('',#9523,#7393,#7394);
#6218=AXIS2_PLACEMENT_3D('',#9524,#7395,#7396);
#6219=AXIS2_PLACEMENT_3D('',#9525,#7397,#7398);
#6220=AXIS2_PLACEMENT_3D('',#9526,#7399,#7400);
#6221=AXIS2_PLACEMENT_3D('',#9527,#7401,#7402);
#6222=AXIS2_PLACEMENT_3D('',#9528,#7403,#7404);
#6223=AXIS2_PLACEMENT_3D('',#9529,#7405,#7406);
#6224=AXIS2_PLACEMENT_3D('',#9530,#7407,#7408);
#6225=AXIS2_PLACEMENT_3D('',#9532,#7409,#7410);
#6226=AXIS2_PLACEMENT_3D('',#9534,#7411,#7412);
#6227=AXIS2_PLACEMENT_3D('',#9535,#7413,#7414);
#6228=AXIS2_PLACEMENT_3D('',#9537,#7415,#7416);
#6229=AXIS2_PLACEMENT_3D('',#9539,#7418,#7419);
#6230=AXIS2_PLACEMENT_3D('',#9541,#7420,#7421);
#6231=AXIS2_PLACEMENT_3D('',#9542,#7422,#7423);
#6232=AXIS2_PLACEMENT_3D('',#9544,#7425,#7426);
#6233=AXIS2_PLACEMENT_3D('',#9546,#7427,#7428);
#6234=AXIS2_PLACEMENT_3D('',#9548,#7429,#7430);
#6235=AXIS2_PLACEMENT_3D('',#9549,#7431,#7432);
#6236=AXIS2_PLACEMENT_3D('',#9551,#7433,#7434);
#6237=AXIS2_PLACEMENT_3D('',#9553,#7436,#7437);
#6238=AXIS2_PLACEMENT_3D('',#9555,#7438,#7439);
#6239=AXIS2_PLACEMENT_3D('',#9556,#7440,#7441);
#6240=AXIS2_PLACEMENT_3D('',#9558,#7443,#7444);
#6241=AXIS2_PLACEMENT_3D('',#9559,#7445,#7446);
#6242=AXIS2_PLACEMENT_3D('',#9560,#7447,#7448);
#6243=AXIS2_PLACEMENT_3D('',#9561,#7449,#7450);
#6244=AXIS2_PLACEMENT_3D('',#9562,#7451,#7452);
#6245=AXIS2_PLACEMENT_3D('',#9563,#7453,#7454);
#6246=AXIS2_PLACEMENT_3D('',#9564,#7455,#7456);
#6247=AXIS2_PLACEMENT_3D('',#9566,#7457,#7458);
#6248=AXIS2_PLACEMENT_3D('',#9567,#7459,#7460);
#6249=AXIS2_PLACEMENT_3D('',#9569,#7461,#7462);
#6250=AXIS2_PLACEMENT_3D('',#9571,#7464,#7465);
#6251=AXIS2_PLACEMENT_3D('',#9573,#7466,#7467);
#6252=AXIS2_PLACEMENT_3D('',#9575,#7469,#7470);
#6253=AXIS2_PLACEMENT_3D('',#9577,#7471,#7472);
#6254=AXIS2_PLACEMENT_3D('',#9579,#7474,#7475);
#6255=AXIS2_PLACEMENT_3D('',#9581,#7476,#7477);
#6256=AXIS2_PLACEMENT_3D('',#9582,#7478,#7479);
#6257=AXIS2_PLACEMENT_3D('',#9584,#7480,#7481);
#6258=AXIS2_PLACEMENT_3D('',#9586,#7483,#7484);
#6259=AXIS2_PLACEMENT_3D('',#9588,#7485,#7486);
#6260=AXIS2_PLACEMENT_3D('',#9590,#7488,#7489);
#6261=AXIS2_PLACEMENT_3D('',#9592,#7490,#7491);
#6262=AXIS2_PLACEMENT_3D('',#9594,#7493,#7494);
#6263=AXIS2_PLACEMENT_3D('',#9595,#7495,#7496);
#6264=AXIS2_PLACEMENT_3D('',#9604,#7501,#7502);
#6265=AXIS2_PLACEMENT_3D('',#9610,#7506,#7507);
#6266=AXIS2_PLACEMENT_3D('',#9616,#7511,#7512);
#6267=AXIS2_PLACEMENT_3D('',#9622,#7516,#7517);
#6268=AXIS2_PLACEMENT_3D('',#9628,#7521,#7522);
#6269=AXIS2_PLACEMENT_3D('',#9631,#7525,#7526);
#6270=AXIS2_PLACEMENT_3D('',#9632,#7527,#7528);
#6271=AXIS2_PLACEMENT_3D('',#9633,#7529,#7530);
#6272=AXIS2_PLACEMENT_3D('',#9634,#7531,#7532);
#6273=AXIS2_PLACEMENT_3D('',#9636,#7533,#7534);
#6274=AXIS2_PLACEMENT_3D('',#9637,#7535,#7536);
#6275=AXIS2_PLACEMENT_3D('',#9639,#7537,#7538);
#6276=AXIS2_PLACEMENT_3D('',#9641,#7540,#7541);
#6277=AXIS2_PLACEMENT_3D('',#9643,#7542,#7543);
#6278=AXIS2_PLACEMENT_3D('',#9645,#7545,#7546);
#6279=AXIS2_PLACEMENT_3D('',#9647,#7547,#7548);
#6280=AXIS2_PLACEMENT_3D('',#9649,#7550,#7551);
#6281=AXIS2_PLACEMENT_3D('',#9651,#7552,#7553);
#6282=AXIS2_PLACEMENT_3D('',#9652,#7554,#7555);
#6283=AXIS2_PLACEMENT_3D('',#9654,#7556,#7557);
#6284=AXIS2_PLACEMENT_3D('',#9656,#7559,#7560);
#6285=AXIS2_PLACEMENT_3D('',#9658,#7561,#7562);
#6286=AXIS2_PLACEMENT_3D('',#9660,#7564,#7565);
#6287=AXIS2_PLACEMENT_3D('',#9662,#7566,#7567);
#6288=AXIS2_PLACEMENT_3D('',#9664,#7569,#7570);
#6289=AXIS2_PLACEMENT_3D('',#9665,#7571,#7572);
#6290=AXIS2_PLACEMENT_3D('',#9674,#7577,#7578);
#6291=AXIS2_PLACEMENT_3D('',#9680,#7582,#7583);
#6292=AXIS2_PLACEMENT_3D('',#9686,#7587,#7588);
#6293=AXIS2_PLACEMENT_3D('',#9692,#7592,#7593);
#6294=AXIS2_PLACEMENT_3D('',#9698,#7597,#7598);
#6295=AXIS2_PLACEMENT_3D('',#9701,#7601,#7602);
#6296=AXIS2_PLACEMENT_3D('',#9702,#7603,#7604);
#6297=AXIS2_PLACEMENT_3D('',#9703,#7605,#7606);
#6298=AXIS2_PLACEMENT_3D('',#9704,#7607,#7608);
#6299=AXIS2_PLACEMENT_3D('',#9705,#7609,#7610);
#6300=AXIS2_PLACEMENT_3D('',#9706,#7611,#7612);
#6301=AXIS2_PLACEMENT_3D('',#9707,#7613,#7614);
#6302=AXIS2_PLACEMENT_3D('',#9708,#7615,#7616);
#6303=AXIS2_PLACEMENT_3D('',#9709,#7617,#7618);
#6304=AXIS2_PLACEMENT_3D('',#9710,#7619,#7620);
#6305=AXIS2_PLACEMENT_3D('',#9711,#7621,#7622);
#6306=AXIS2_PLACEMENT_3D('',#9712,#7623,#7624);
#6307=AXIS2_PLACEMENT_3D('',#9713,#7625,#7626);
#6308=AXIS2_PLACEMENT_3D('',#9714,#7627,#7628);
#6309=AXIS2_PLACEMENT_3D('',#9715,#7629,#7630);
#6310=AXIS2_PLACEMENT_3D('',#9716,#7631,#7632);
#6311=AXIS2_PLACEMENT_3D('',#9717,#7633,#7634);
#6312=AXIS2_PLACEMENT_3D('',#9718,#7635,#7636);
#6313=AXIS2_PLACEMENT_3D('',#9719,#7637,#7638);
#6314=AXIS2_PLACEMENT_3D('',#9720,#7639,#7640);
#6315=AXIS2_PLACEMENT_3D('',#9721,#7641,#7642);
#6316=AXIS2_PLACEMENT_3D('',#9722,#7643,#7644);
#6317=AXIS2_PLACEMENT_3D('',#9723,#7645,#7646);
#6318=AXIS2_PLACEMENT_3D('',#9724,#7647,#7648);
#6319=AXIS2_PLACEMENT_3D('',#9725,#7649,#7650);
#6320=AXIS2_PLACEMENT_3D('',#9726,#7651,#7652);
#6321=AXIS2_PLACEMENT_3D('',#9727,#7653,#7654);
#6322=AXIS2_PLACEMENT_3D('',#9736,#7659,#7660);
#6323=AXIS2_PLACEMENT_3D('',#9738,#7661,#7662);
#6324=AXIS2_PLACEMENT_3D('',#9742,#7665,#7666);
#6325=AXIS2_PLACEMENT_3D('',#9748,#7670,#7671);
#6326=AXIS2_PLACEMENT_3D('',#9750,#7673,#7674);
#6327=AXIS2_PLACEMENT_3D('',#9751,#7675,#7676);
#6328=AXIS2_PLACEMENT_3D('',#9752,#7677,#7678);
#6329=AXIS2_PLACEMENT_3D('',#9754,#7679,#7680);
#6330=AXIS2_PLACEMENT_3D('',#9757,#7682,#7683);
#6331=AXIS2_PLACEMENT_3D('',#9758,#7684,#7685);
#6332=AXIS2_PLACEMENT_3D('',#9759,#7686,#7687);
#6333=AXIS2_PLACEMENT_3D('',#9761,#7688,#7689);
#6334=AXIS2_PLACEMENT_3D('',#9763,#7690,#7691);
#6335=AXIS2_PLACEMENT_3D('',#9764,#7692,#7693);
#6336=AXIS2_PLACEMENT_3D('',#9766,#7694,#7695);
#6337=AXIS2_PLACEMENT_3D('',#9768,#7696,#7697);
#6338=AXIS2_PLACEMENT_3D('',#9769,#7698,#7699);
#6339=AXIS2_PLACEMENT_3D('',#9771,#7701,#7702);
#6340=AXIS2_PLACEMENT_3D('',#9774,#7704,#7705);
#6341=AXIS2_PLACEMENT_3D('',#9775,#7706,#7707);
#6342=AXIS2_PLACEMENT_3D('',#9777,#7708,#7709);
#6343=AXIS2_PLACEMENT_3D('',#9779,#7711,#7712);
#6344=AXIS2_PLACEMENT_3D('',#9780,#7713,#7714);
#6345=AXIS2_PLACEMENT_3D('',#9781,#7715,#7716);
#6346=AXIS2_PLACEMENT_3D('',#9782,#7717,#7718);
#6347=AXIS2_PLACEMENT_3D('',#9784,#7719,#7720);
#6348=AXIS2_PLACEMENT_3D('',#9787,#7722,#7723);
#6349=AXIS2_PLACEMENT_3D('',#9788,#7724,#7725);
#6350=AXIS2_PLACEMENT_3D('',#9790,#7726,#7727);
#6351=AXIS2_PLACEMENT_3D('',#9793,#7729,#7730);
#6352=AXIS2_PLACEMENT_3D('',#9794,#7731,#7732);
#6353=AXIS2_PLACEMENT_3D('',#9795,#7733,#7734);
#6354=AXIS2_PLACEMENT_3D('',#9796,#7735,#7736);
#6355=AXIS2_PLACEMENT_3D('',#9797,#7737,#7738);
#6356=AXIS2_PLACEMENT_3D('',#9801,#7740,#7741);
#6357=AXIS2_PLACEMENT_3D('',#9802,#7742,#7743);
#6358=AXIS2_PLACEMENT_3D('',#9819,#7744,#7745);
#6359=AXIS2_PLACEMENT_3D('',#9860,#7747,#7748);
#6360=AXIS2_PLACEMENT_3D('',#9875,#7749,#7750);
#6361=AXIS2_PLACEMENT_3D('',#9877,#7752,#7753);
#6362=AXIS2_PLACEMENT_3D('',#9879,#7754,#7755);
#6363=AXIS2_PLACEMENT_3D('',#9882,#7757,#7758);
#6364=AXIS2_PLACEMENT_3D('',#9883,#7759,#7760);
#6365=AXIS2_PLACEMENT_3D('',#9885,#7761,#7762);
#6366=AXIS2_PLACEMENT_3D('',#9888,#7764,#7765);
#6367=AXIS2_PLACEMENT_3D('',#9889,#7766,#7767);
#6368=AXIS2_PLACEMENT_3D('',#9890,#7768,#7769);
#6369=AXIS2_PLACEMENT_3D('',#9891,#7770,#7771);
#6370=AXIS2_PLACEMENT_3D('',#9892,#7772,#7773);
#6371=AXIS2_PLACEMENT_3D('',#9896,#7775,#7776);
#6372=AXIS2_PLACEMENT_3D('',#9897,#7777,#7778);
#6373=AXIS2_PLACEMENT_3D('',#9910,#7779,#7780);
#6374=AXIS2_PLACEMENT_3D('',#9951,#7782,#7783);
#6375=AXIS2_PLACEMENT_3D('',#9962,#7784,#7785);
#6376=AXIS2_PLACEMENT_3D('',#9964,#7787,#7788);
#6377=AXIS2_PLACEMENT_3D('',#9966,#7789,#7790);
#6378=AXIS2_PLACEMENT_3D('',#9969,#7792,#7793);
#6379=AXIS2_PLACEMENT_3D('',#9970,#7794,#7795);
#6380=AXIS2_PLACEMENT_3D('',#9972,#7796,#7797);
#6381=AXIS2_PLACEMENT_3D('',#9975,#7799,#7800);
#6382=AXIS2_PLACEMENT_3D('',#9976,#7801,#7802);
#6383=AXIS2_PLACEMENT_3D('',#9977,#7803,#7804);
#6384=AXIS2_PLACEMENT_3D('',#9978,#7805,#7806);
#6385=AXIS2_PLACEMENT_3D('',#9979,#7807,#7808);
#6386=AXIS2_PLACEMENT_3D('',#9988,#7813,#7814);
#6387=AXIS2_PLACEMENT_3D('',#9995,#7818,#7819);
#6388=AXIS2_PLACEMENT_3D('',#9996,#7820,#7821);
#6389=AXIS2_PLACEMENT_3D('',#10002,#7825,#7826);
#6390=AXIS2_PLACEMENT_3D('',#10004,#7827,#7828);
#6391=AXIS2_PLACEMENT_3D('',#10005,#7829,#7830);
#6392=AXIS2_PLACEMENT_3D('',#10006,#7831,#7832);
#6393=AXIS2_PLACEMENT_3D('',#10007,#7833,#7834);
#6394=AXIS2_PLACEMENT_3D('',#10122,#7835,#7836);
#6395=AXIS2_PLACEMENT_3D('',#10165,#7838,#7839);
#6396=AXIS2_PLACEMENT_3D('',#10208,#7841,#7842);
#6397=AXIS2_PLACEMENT_3D('',#10210,#7843,#7844);
#6398=AXIS2_PLACEMENT_3D('',#10214,#7847,#7848);
#6399=AXIS2_PLACEMENT_3D('',#10297,#7849,#7850);
#6400=AXIS2_PLACEMENT_3D('',#10299,#7852,#7853);
#6401=AXIS2_PLACEMENT_3D('',#10301,#7855,#7856);
#6402=AXIS2_PLACEMENT_3D('',#10302,#7857,#7858);
#6403=AXIS2_PLACEMENT_3D('',#10304,#7859,#7860);
#6404=AXIS2_PLACEMENT_3D('',#10307,#7861,#7862);
#6405=AXIS2_PLACEMENT_3D('',#10309,#7863,#7864);
#6406=AXIS2_PLACEMENT_3D('',#10311,#7865,#7866);
#6407=AXIS2_PLACEMENT_3D('',#10313,#7867,#7868);
#6408=AXIS2_PLACEMENT_3D('',#10315,#7869,#7870);
#6409=AXIS2_PLACEMENT_3D('',#10317,#7871,#7872);
#6410=AXIS2_PLACEMENT_3D('',#10319,#7873,#7874);
#6411=AXIS2_PLACEMENT_3D('',#10321,#7875,#7876);
#6412=AXIS2_PLACEMENT_3D('',#10323,#7877,#7878);
#6413=AXIS2_PLACEMENT_3D('',#10325,#7879,#7880);
#6414=AXIS2_PLACEMENT_3D('',#10327,#7881,#7882);
#6415=AXIS2_PLACEMENT_3D('',#10329,#7883,#7884);
#6416=AXIS2_PLACEMENT_3D('',#10331,#7885,#7886);
#6417=AXIS2_PLACEMENT_3D('',#10333,#7887,#7888);
#6418=AXIS2_PLACEMENT_3D('',#10335,#7889,#7890);
#6419=AXIS2_PLACEMENT_3D('',#10337,#7891,#7892);
#6420=AXIS2_PLACEMENT_3D('',#10339,#7893,#7894);
#6421=AXIS2_PLACEMENT_3D('',#10341,#7895,#7896);
#6422=AXIS2_PLACEMENT_3D('',#10343,#7897,#7898);
#6423=AXIS2_PLACEMENT_3D('',#10345,#7899,#7900);
#6424=AXIS2_PLACEMENT_3D('',#10347,#7901,#7902);
#6425=AXIS2_PLACEMENT_3D('',#10349,#7903,#7904);
#6426=AXIS2_PLACEMENT_3D('',#10351,#7905,#7906);
#6427=AXIS2_PLACEMENT_3D('',#10353,#7907,#7908);
#6428=AXIS2_PLACEMENT_3D('',#10355,#7909,#7910);
#6429=AXIS2_PLACEMENT_3D('',#10357,#7911,#7912);
#6430=AXIS2_PLACEMENT_3D('',#10359,#7913,#7914);
#6431=AXIS2_PLACEMENT_3D('',#10361,#7915,#7916);
#6432=AXIS2_PLACEMENT_3D('',#10363,#7917,#7918);
#6433=AXIS2_PLACEMENT_3D('',#10365,#7919,#7920);
#6434=AXIS2_PLACEMENT_3D('',#10367,#7921,#7922);
#6435=AXIS2_PLACEMENT_3D('',#10369,#7923,#7924);
#6436=AXIS2_PLACEMENT_3D('',#10371,#7925,#7926);
#6437=AXIS2_PLACEMENT_3D('',#10373,#7927,#7928);
#6438=AXIS2_PLACEMENT_3D('',#10375,#7929,#7930);
#6439=AXIS2_PLACEMENT_3D('',#10377,#7931,#7932);
#6440=AXIS2_PLACEMENT_3D('',#10379,#7933,#7934);
#6441=AXIS2_PLACEMENT_3D('',#10381,#7935,#7936);
#6442=AXIS2_PLACEMENT_3D('',#10383,#7937,#7938);
#6443=AXIS2_PLACEMENT_3D('',#10385,#7939,#7940);
#6444=AXIS2_PLACEMENT_3D('',#10387,#7941,#7942);
#6445=AXIS2_PLACEMENT_3D('',#10389,#7943,#7944);
#6446=AXIS2_PLACEMENT_3D('',#10391,#7945,#7946);
#6447=AXIS2_PLACEMENT_3D('',#10393,#7947,#7948);
#6448=AXIS2_PLACEMENT_3D('',#10395,#7949,#7950);
#6449=AXIS2_PLACEMENT_3D('',#10397,#7951,#7952);
#6450=AXIS2_PLACEMENT_3D('',#10399,#7953,#7954);
#6451=AXIS2_PLACEMENT_3D('',#10401,#7955,#7956);
#6452=AXIS2_PLACEMENT_3D('',#10403,#7957,#7958);
#6453=AXIS2_PLACEMENT_3D('',#10405,#7959,#7960);
#6454=AXIS2_PLACEMENT_3D('',#10407,#7961,#7962);
#6455=AXIS2_PLACEMENT_3D('',#10409,#7963,#7964);
#6456=AXIS2_PLACEMENT_3D('',#10411,#7965,#7966);
#6457=AXIS2_PLACEMENT_3D('',#10413,#7967,#7968);
#6458=AXIS2_PLACEMENT_3D('',#10415,#7969,#7970);
#6459=AXIS2_PLACEMENT_3D('',#10417,#7971,#7972);
#6460=AXIS2_PLACEMENT_3D('',#10419,#7973,#7974);
#6461=AXIS2_PLACEMENT_3D('',#10421,#7975,#7976);
#6462=AXIS2_PLACEMENT_3D('',#10423,#7977,#7978);
#6463=AXIS2_PLACEMENT_3D('',#10425,#7979,#7980);
#6464=AXIS2_PLACEMENT_3D('',#10427,#7981,#7982);
#6465=AXIS2_PLACEMENT_3D('',#10429,#7983,#7984);
#6466=AXIS2_PLACEMENT_3D('',#10431,#7985,#7986);
#6467=AXIS2_PLACEMENT_3D('',#10433,#7987,#7988);
#6468=AXIS2_PLACEMENT_3D('',#10435,#7989,#7990);
#6469=AXIS2_PLACEMENT_3D('',#10437,#7991,#7992);
#6470=AXIS2_PLACEMENT_3D('',#10439,#7993,#7994);
#6471=AXIS2_PLACEMENT_3D('',#10441,#7995,#7996);
#6472=AXIS2_PLACEMENT_3D('',#10443,#7997,#7998);
#6473=AXIS2_PLACEMENT_3D('',#10445,#7999,#8000);
#6474=AXIS2_PLACEMENT_3D('',#10447,#8001,#8002);
#6475=AXIS2_PLACEMENT_3D('',#10449,#8003,#8004);
#6476=AXIS2_PLACEMENT_3D('',#10451,#8005,#8006);
#6477=AXIS2_PLACEMENT_3D('',#10453,#8007,#8008);
#6478=AXIS2_PLACEMENT_3D('',#10455,#8009,#8010);
#6479=AXIS2_PLACEMENT_3D('',#10457,#8011,#8012);
#6480=AXIS2_PLACEMENT_3D('',#10459,#8013,#8014);
#6481=AXIS2_PLACEMENT_3D('',#10461,#8015,#8016);
#6482=AXIS2_PLACEMENT_3D('',#10463,#8017,#8018);
#6483=AXIS2_PLACEMENT_3D('',#10464,#8019,#8020);
#6484=AXIS2_PLACEMENT_3D('',#10465,#8021,#8022);
#6485=AXIS2_PLACEMENT_3D('',#10467,#8023,#8024);
#6486=AXIS2_PLACEMENT_3D('',#10469,#8026,#8027);
#6487=AXIS2_PLACEMENT_3D('',#10470,#8028,#8029);
#6488=AXIS2_PLACEMENT_3D('',#10472,#8030,#8031);
#6489=AXIS2_PLACEMENT_3D('',#10475,#8032,#8033);
#6490=AXIS2_PLACEMENT_3D('',#10477,#8034,#8035);
#6491=AXIS2_PLACEMENT_3D('',#10479,#8036,#8037);
#6492=AXIS2_PLACEMENT_3D('',#10481,#8038,#8039);
#6493=AXIS2_PLACEMENT_3D('',#10483,#8040,#8041);
#6494=AXIS2_PLACEMENT_3D('',#10485,#8042,#8043);
#6495=AXIS2_PLACEMENT_3D('',#10487,#8044,#8045);
#6496=AXIS2_PLACEMENT_3D('',#10489,#8046,#8047);
#6497=AXIS2_PLACEMENT_3D('',#10491,#8048,#8049);
#6498=AXIS2_PLACEMENT_3D('',#10493,#8050,#8051);
#6499=AXIS2_PLACEMENT_3D('',#10495,#8052,#8053);
#6500=AXIS2_PLACEMENT_3D('',#10497,#8054,#8055);
#6501=AXIS2_PLACEMENT_3D('',#10499,#8056,#8057);
#6502=AXIS2_PLACEMENT_3D('',#10501,#8058,#8059);
#6503=AXIS2_PLACEMENT_3D('',#10503,#8060,#8061);
#6504=AXIS2_PLACEMENT_3D('',#10505,#8062,#8063);
#6505=AXIS2_PLACEMENT_3D('',#10507,#8064,#8065);
#6506=AXIS2_PLACEMENT_3D('',#10509,#8066,#8067);
#6507=AXIS2_PLACEMENT_3D('',#10511,#8068,#8069);
#6508=AXIS2_PLACEMENT_3D('',#10513,#8070,#8071);
#6509=AXIS2_PLACEMENT_3D('',#10515,#8072,#8073);
#6510=AXIS2_PLACEMENT_3D('',#10517,#8074,#8075);
#6511=AXIS2_PLACEMENT_3D('',#10519,#8076,#8077);
#6512=AXIS2_PLACEMENT_3D('',#10521,#8078,#8079);
#6513=AXIS2_PLACEMENT_3D('',#10523,#8080,#8081);
#6514=AXIS2_PLACEMENT_3D('',#10525,#8082,#8083);
#6515=AXIS2_PLACEMENT_3D('',#10527,#8084,#8085);
#6516=AXIS2_PLACEMENT_3D('',#10529,#8086,#8087);
#6517=AXIS2_PLACEMENT_3D('',#10531,#8088,#8089);
#6518=AXIS2_PLACEMENT_3D('',#10533,#8090,#8091);
#6519=AXIS2_PLACEMENT_3D('',#10535,#8092,#8093);
#6520=AXIS2_PLACEMENT_3D('',#10537,#8094,#8095);
#6521=AXIS2_PLACEMENT_3D('',#10539,#8096,#8097);
#6522=AXIS2_PLACEMENT_3D('',#10541,#8098,#8099);
#6523=AXIS2_PLACEMENT_3D('',#10543,#8100,#8101);
#6524=AXIS2_PLACEMENT_3D('',#10545,#8102,#8103);
#6525=AXIS2_PLACEMENT_3D('',#10547,#8104,#8105);
#6526=AXIS2_PLACEMENT_3D('',#10549,#8106,#8107);
#6527=AXIS2_PLACEMENT_3D('',#10551,#8108,#8109);
#6528=AXIS2_PLACEMENT_3D('',#10553,#8110,#8111);
#6529=AXIS2_PLACEMENT_3D('',#10555,#8112,#8113);
#6530=AXIS2_PLACEMENT_3D('',#10557,#8114,#8115);
#6531=AXIS2_PLACEMENT_3D('',#10559,#8116,#8117);
#6532=AXIS2_PLACEMENT_3D('',#10561,#8118,#8119);
#6533=AXIS2_PLACEMENT_3D('',#10563,#8120,#8121);
#6534=AXIS2_PLACEMENT_3D('',#10565,#8122,#8123);
#6535=AXIS2_PLACEMENT_3D('',#10567,#8124,#8125);
#6536=AXIS2_PLACEMENT_3D('',#10569,#8126,#8127);
#6537=AXIS2_PLACEMENT_3D('',#10571,#8128,#8129);
#6538=AXIS2_PLACEMENT_3D('',#10573,#8130,#8131);
#6539=AXIS2_PLACEMENT_3D('',#10575,#8132,#8133);
#6540=AXIS2_PLACEMENT_3D('',#10577,#8134,#8135);
#6541=AXIS2_PLACEMENT_3D('',#10579,#8136,#8137);
#6542=AXIS2_PLACEMENT_3D('',#10581,#8138,#8139);
#6543=AXIS2_PLACEMENT_3D('',#10583,#8140,#8141);
#6544=AXIS2_PLACEMENT_3D('',#10585,#8142,#8143);
#6545=AXIS2_PLACEMENT_3D('',#10587,#8144,#8145);
#6546=AXIS2_PLACEMENT_3D('',#10589,#8146,#8147);
#6547=AXIS2_PLACEMENT_3D('',#10591,#8148,#8149);
#6548=AXIS2_PLACEMENT_3D('',#10593,#8150,#8151);
#6549=AXIS2_PLACEMENT_3D('',#10595,#8152,#8153);
#6550=AXIS2_PLACEMENT_3D('',#10597,#8154,#8155);
#6551=AXIS2_PLACEMENT_3D('',#10599,#8156,#8157);
#6552=AXIS2_PLACEMENT_3D('',#10601,#8158,#8159);
#6553=AXIS2_PLACEMENT_3D('',#10603,#8160,#8161);
#6554=AXIS2_PLACEMENT_3D('',#10605,#8162,#8163);
#6555=AXIS2_PLACEMENT_3D('',#10607,#8164,#8165);
#6556=AXIS2_PLACEMENT_3D('',#10609,#8166,#8167);
#6557=AXIS2_PLACEMENT_3D('',#10611,#8168,#8169);
#6558=AXIS2_PLACEMENT_3D('',#10613,#8170,#8171);
#6559=AXIS2_PLACEMENT_3D('',#10615,#8172,#8173);
#6560=AXIS2_PLACEMENT_3D('',#10617,#8174,#8175);
#6561=AXIS2_PLACEMENT_3D('',#10619,#8176,#8177);
#6562=AXIS2_PLACEMENT_3D('',#10621,#8178,#8179);
#6563=AXIS2_PLACEMENT_3D('',#10623,#8180,#8181);
#6564=AXIS2_PLACEMENT_3D('',#10625,#8182,#8183);
#6565=AXIS2_PLACEMENT_3D('',#10627,#8184,#8185);
#6566=AXIS2_PLACEMENT_3D('',#10629,#8186,#8187);
#6567=AXIS2_PLACEMENT_3D('',#10631,#8188,#8189);
#6568=AXIS2_PLACEMENT_3D('',#10632,#8190,#8191);
#6569=AXIS2_PLACEMENT_3D('',#10633,#8192,#8193);
#6570=AXIS2_PLACEMENT_3D('',#10635,#8195,#8196);
#6571=AXIS2_PLACEMENT_3D('',#10638,#8199,#8200);
#6572=AXIS2_PLACEMENT_3D('',#10640,#8202,#8203);
#6573=AXIS2_PLACEMENT_3D('',#10642,#8205,#8206);
#6574=AXIS2_PLACEMENT_3D('',#10644,#8208,#8209);
#6575=AXIS2_PLACEMENT_3D('',#10646,#8211,#8212);
#6576=AXIS2_PLACEMENT_3D('',#10648,#8214,#8215);
#6577=AXIS2_PLACEMENT_3D('',#10650,#8217,#8218);
#6578=AXIS2_PLACEMENT_3D('',#10652,#8220,#8221);
#6579=AXIS2_PLACEMENT_3D('',#10654,#8223,#8224);
#6580=AXIS2_PLACEMENT_3D('',#10656,#8226,#8227);
#6581=AXIS2_PLACEMENT_3D('',#10658,#8229,#8230);
#6582=AXIS2_PLACEMENT_3D('',#10660,#8232,#8233);
#6583=AXIS2_PLACEMENT_3D('',#10662,#8235,#8236);
#6584=AXIS2_PLACEMENT_3D('',#10664,#8238,#8239);
#6585=AXIS2_PLACEMENT_3D('',#10666,#8241,#8242);
#6586=AXIS2_PLACEMENT_3D('',#10668,#8244,#8245);
#6587=AXIS2_PLACEMENT_3D('',#10670,#8247,#8248);
#6588=AXIS2_PLACEMENT_3D('',#10672,#8250,#8251);
#6589=AXIS2_PLACEMENT_3D('',#10674,#8253,#8254);
#6590=AXIS2_PLACEMENT_3D('',#10676,#8256,#8257);
#6591=AXIS2_PLACEMENT_3D('',#10678,#8259,#8260);
#6592=AXIS2_PLACEMENT_3D('',#10680,#8262,#8263);
#6593=AXIS2_PLACEMENT_3D('',#10682,#8265,#8266);
#6594=AXIS2_PLACEMENT_3D('',#10684,#8268,#8269);
#6595=AXIS2_PLACEMENT_3D('',#10686,#8271,#8272);
#6596=AXIS2_PLACEMENT_3D('',#10688,#8274,#8275);
#6597=AXIS2_PLACEMENT_3D('',#10690,#8277,#8278);
#6598=AXIS2_PLACEMENT_3D('',#10692,#8280,#8281);
#6599=AXIS2_PLACEMENT_3D('',#10694,#8283,#8284);
#6600=AXIS2_PLACEMENT_3D('',#10696,#8286,#8287);
#6601=AXIS2_PLACEMENT_3D('',#10698,#8289,#8290);
#6602=AXIS2_PLACEMENT_3D('',#10700,#8292,#8293);
#6603=AXIS2_PLACEMENT_3D('',#10702,#8295,#8296);
#6604=AXIS2_PLACEMENT_3D('',#10704,#8298,#8299);
#6605=AXIS2_PLACEMENT_3D('',#10706,#8301,#8302);
#6606=AXIS2_PLACEMENT_3D('',#10708,#8304,#8305);
#6607=AXIS2_PLACEMENT_3D('',#10710,#8307,#8308);
#6608=AXIS2_PLACEMENT_3D('',#10712,#8310,#8311);
#6609=AXIS2_PLACEMENT_3D('',#10714,#8313,#8314);
#6610=AXIS2_PLACEMENT_3D('',#10716,#8316,#8317);
#6611=AXIS2_PLACEMENT_3D('',#10718,#8319,#8320);
#6612=AXIS2_PLACEMENT_3D('',#10720,#8322,#8323);
#6613=AXIS2_PLACEMENT_3D('',#10722,#8325,#8326);
#6614=AXIS2_PLACEMENT_3D('',#10724,#8328,#8329);
#6615=AXIS2_PLACEMENT_3D('',#10726,#8331,#8332);
#6616=AXIS2_PLACEMENT_3D('',#10728,#8334,#8335);
#6617=AXIS2_PLACEMENT_3D('',#10730,#8337,#8338);
#6618=AXIS2_PLACEMENT_3D('',#10732,#8340,#8341);
#6619=AXIS2_PLACEMENT_3D('',#10734,#8343,#8344);
#6620=AXIS2_PLACEMENT_3D('',#10736,#8346,#8347);
#6621=AXIS2_PLACEMENT_3D('',#10738,#8349,#8350);
#6622=AXIS2_PLACEMENT_3D('',#10740,#8352,#8353);
#6623=AXIS2_PLACEMENT_3D('',#10742,#8355,#8356);
#6624=AXIS2_PLACEMENT_3D('',#10744,#8358,#8359);
#6625=AXIS2_PLACEMENT_3D('',#10746,#8361,#8362);
#6626=AXIS2_PLACEMENT_3D('',#10748,#8364,#8365);
#6627=AXIS2_PLACEMENT_3D('',#10750,#8367,#8368);
#6628=AXIS2_PLACEMENT_3D('',#10752,#8370,#8371);
#6629=AXIS2_PLACEMENT_3D('',#10754,#8373,#8374);
#6630=AXIS2_PLACEMENT_3D('',#10756,#8376,#8377);
#6631=AXIS2_PLACEMENT_3D('',#10758,#8379,#8380);
#6632=AXIS2_PLACEMENT_3D('',#10760,#8382,#8383);
#6633=AXIS2_PLACEMENT_3D('',#10762,#8385,#8386);
#6634=AXIS2_PLACEMENT_3D('',#10764,#8388,#8389);
#6635=AXIS2_PLACEMENT_3D('',#10766,#8391,#8392);
#6636=AXIS2_PLACEMENT_3D('',#10768,#8394,#8395);
#6637=AXIS2_PLACEMENT_3D('',#10770,#8397,#8398);
#6638=AXIS2_PLACEMENT_3D('',#10772,#8400,#8401);
#6639=AXIS2_PLACEMENT_3D('',#10774,#8403,#8404);
#6640=AXIS2_PLACEMENT_3D('',#10776,#8406,#8407);
#6641=AXIS2_PLACEMENT_3D('',#10778,#8409,#8410);
#6642=AXIS2_PLACEMENT_3D('',#10780,#8412,#8413);
#6643=AXIS2_PLACEMENT_3D('',#10782,#8415,#8416);
#6644=AXIS2_PLACEMENT_3D('',#10784,#8418,#8419);
#6645=AXIS2_PLACEMENT_3D('',#10786,#8421,#8422);
#6646=AXIS2_PLACEMENT_3D('',#10788,#8424,#8425);
#6647=AXIS2_PLACEMENT_3D('',#10790,#8427,#8428);
#6648=AXIS2_PLACEMENT_3D('',#10792,#8430,#8431);
#6649=AXIS2_PLACEMENT_3D('',#10794,#8433,#8434);
#6650=AXIS2_PLACEMENT_3D('',#10795,#8435,#8436);
#6651=AXIS2_PLACEMENT_3D('',#10796,#8437,#8438);
#6652=AXIS2_PLACEMENT_3D('',#10813,#8447,#8448);
#6653=AXIS2_PLACEMENT_3D('',#10819,#8452,#8453);
#6654=AXIS2_PLACEMENT_3D('',#10823,#8456,#8457);
#6655=AXIS2_PLACEMENT_3D('',#10827,#8460,#8461);
#6656=AXIS2_PLACEMENT_3D('',#10831,#8464,#8465);
#6657=AXIS2_PLACEMENT_3D('',#10839,#8470,#8471);
#6658=AXIS2_PLACEMENT_3D('',#10841,#8473,#8474);
#6659=AXIS2_PLACEMENT_3D('',#10843,#8476,#8477);
#6660=AXIS2_PLACEMENT_3D('',#10845,#8479,#8480);
#6661=AXIS2_PLACEMENT_3D('',#10846,#8481,#8482);
#6662=AXIS2_PLACEMENT_3D('',#10847,#8483,#8484);
#6663=AXIS2_PLACEMENT_3D('',#10856,#8489,#8490);
#6664=AXIS2_PLACEMENT_3D('',#10862,#8494,#8495);
#6665=AXIS2_PLACEMENT_3D('',#10868,#8499,#8500);
#6666=AXIS2_PLACEMENT_3D('',#10874,#8504,#8505);
#6667=AXIS2_PLACEMENT_3D('',#10880,#8509,#8510);
#6668=AXIS2_PLACEMENT_3D('',#10883,#8513,#8514);
#6669=AXIS2_PLACEMENT_3D('',#10884,#8515,#8516);
#6670=AXIS2_PLACEMENT_3D('',#10886,#8517,#8518);
#6671=AXIS2_PLACEMENT_3D('',#10887,#8519,#8520);
#6672=AXIS2_PLACEMENT_3D('',#10889,#8521,#8522);
#6673=AXIS2_PLACEMENT_3D('',#10891,#8524,#8525);
#6674=AXIS2_PLACEMENT_3D('',#10893,#8526,#8527);
#6675=AXIS2_PLACEMENT_3D('',#10895,#8529,#8530);
#6676=AXIS2_PLACEMENT_3D('',#10897,#8531,#8532);
#6677=AXIS2_PLACEMENT_3D('',#10899,#8534,#8535);
#6678=AXIS2_PLACEMENT_3D('',#10900,#8536,#8537);
#6679=AXIS2_PLACEMENT_3D('',#10901,#8538,#8539);
#6680=AXIS2_PLACEMENT_3D('',#10902,#8540,#8541);
#6681=AXIS2_PLACEMENT_3D('',#10903,#8542,#8543);
#6682=AXIS2_PLACEMENT_3D('',#10904,#8544,#8545);
#6683=AXIS2_PLACEMENT_3D('',#10905,#8546,#8547);
#6684=AXIS2_PLACEMENT_3D('',#10906,#8548,#8549);
#6685=AXIS2_PLACEMENT_3D('',#10907,#8550,#8551);
#6686=AXIS2_PLACEMENT_3D('',#10908,#8552,#8553);
#6687=AXIS2_PLACEMENT_3D('',#10909,#8554,#8555);
#6688=DIRECTION('axis',(0.,0.,1.));
#6689=DIRECTION('refdir',(1.,0.,0.));
#6690=DIRECTION('axis',(0.,0.,1.));
#6691=DIRECTION('refdir',(1.,0.,0.));
#6692=DIRECTION('axis',(0.,0.,1.));
#6693=DIRECTION('refdir',(1.,0.,0.));
#6694=DIRECTION('center_axis',(0.,0.,1.));
#6695=DIRECTION('ref_axis',(1.,0.,0.));
#6696=DIRECTION('center_axis',(0.,0.,1.));
#6697=DIRECTION('ref_axis',(1.,0.,0.));
#6698=DIRECTION('',(0.,0.,1.));
#6699=DIRECTION('center_axis',(0.,0.,-1.));
#6700=DIRECTION('ref_axis',(1.,0.,0.));
#6701=DIRECTION('center_axis',(0.,0.,1.));
#6702=DIRECTION('ref_axis',(1.,0.,0.));
#6703=DIRECTION('center_axis',(0.,0.,1.));
#6704=DIRECTION('ref_axis',(1.,0.,0.));
#6705=DIRECTION('',(0.,0.,1.));
#6706=DIRECTION('center_axis',(0.,0.,-1.));
#6707=DIRECTION('ref_axis',(1.,0.,0.));
#6708=DIRECTION('center_axis',(0.,0.,1.));
#6709=DIRECTION('ref_axis',(1.,0.,0.));
#6710=DIRECTION('center_axis',(0.,0.,1.));
#6711=DIRECTION('ref_axis',(1.,0.,0.));
#6712=DIRECTION('',(0.,0.,1.));
#6713=DIRECTION('center_axis',(0.,0.,-1.));
#6714=DIRECTION('ref_axis',(1.,0.,0.));
#6715=DIRECTION('center_axis',(0.,0.,1.));
#6716=DIRECTION('ref_axis',(1.,0.,0.));
#6717=DIRECTION('center_axis',(0.,0.,1.));
#6718=DIRECTION('ref_axis',(1.,0.,0.));
#6719=DIRECTION('',(0.,0.,1.));
#6720=DIRECTION('center_axis',(0.,0.,-1.));
#6721=DIRECTION('ref_axis',(1.,0.,0.));
#6722=DIRECTION('center_axis',(0.,1.,0.));
#6723=DIRECTION('ref_axis',(-1.,0.,0.));
#6724=DIRECTION('',(-1.,0.,0.));
#6725=DIRECTION('',(0.,0.,1.));
#6726=DIRECTION('',(-1.,0.,0.));
#6727=DIRECTION('',(0.,0.,1.));
#6728=DIRECTION('center_axis',(1.,0.,0.));
#6729=DIRECTION('ref_axis',(0.,1.,0.));
#6730=DIRECTION('',(0.,1.,0.));
#6731=DIRECTION('',(0.,1.,0.));
#6732=DIRECTION('',(0.,0.,1.));
#6733=DIRECTION('center_axis',(0.,-1.,0.));
#6734=DIRECTION('ref_axis',(1.,0.,0.));
#6735=DIRECTION('',(1.,0.,0.));
#6736=DIRECTION('',(1.,0.,0.));
#6737=DIRECTION('',(0.,0.,1.));
#6738=DIRECTION('center_axis',(-1.,0.,0.));
#6739=DIRECTION('ref_axis',(0.,-1.,0.));
#6740=DIRECTION('',(0.,-1.,0.));
#6741=DIRECTION('',(0.,-1.,0.));
#6742=DIRECTION('center_axis',(0.,0.,1.));
#6743=DIRECTION('ref_axis',(1.,0.,0.));
#6744=DIRECTION('center_axis',(0.,0.,1.));
#6745=DIRECTION('ref_axis',(1.,0.,0.));
#6746=DIRECTION('axis',(0.,0.,1.));
#6747=DIRECTION('refdir',(1.,0.,0.));
#6748=DIRECTION('center_axis',(0.,1.,0.));
#6749=DIRECTION('ref_axis',(1.,0.,0.));
#6750=DIRECTION('center_axis',(0.,1.,0.));
#6751=DIRECTION('ref_axis',(1.,0.,0.));
#6752=DIRECTION('',(0.,1.,0.));
#6753=DIRECTION('center_axis',(0.,-1.,0.));
#6754=DIRECTION('ref_axis',(1.,0.,0.));
#6755=DIRECTION('center_axis',(0.,1.,0.));
#6756=DIRECTION('ref_axis',(1.,0.,0.));
#6757=DIRECTION('center_axis',(0.,1.,0.));
#6758=DIRECTION('ref_axis',(1.,0.,0.));
#6759=DIRECTION('center_axis',(0.,1.,0.));
#6760=DIRECTION('ref_axis',(1.,0.,0.));
#6761=DIRECTION('',(0.,1.,0.));
#6762=DIRECTION('center_axis',(0.,-1.,0.));
#6763=DIRECTION('ref_axis',(1.,0.,0.));
#6764=DIRECTION('center_axis',(0.,1.,0.));
#6765=DIRECTION('ref_axis',(1.,0.,0.));
#6766=DIRECTION('center_axis',(0.,1.,0.));
#6767=DIRECTION('ref_axis',(1.,0.,0.));
#6768=DIRECTION('center_axis',(0.,1.,0.));
#6769=DIRECTION('ref_axis',(1.,0.,0.));
#6770=DIRECTION('',(0.,1.,0.));
#6771=DIRECTION('center_axis',(0.,-1.,0.));
#6772=DIRECTION('ref_axis',(1.,0.,0.));
#6773=DIRECTION('center_axis',(0.,1.,0.));
#6774=DIRECTION('ref_axis',(1.,0.,0.));
#6775=DIRECTION('center_axis',(0.,1.,0.));
#6776=DIRECTION('ref_axis',(1.,0.,0.));
#6777=DIRECTION('center_axis',(0.,1.,0.));
#6778=DIRECTION('ref_axis',(1.,0.,0.));
#6779=DIRECTION('',(0.,1.,0.));
#6780=DIRECTION('center_axis',(0.,-1.,0.));
#6781=DIRECTION('ref_axis',(1.,0.,0.));
#6782=DIRECTION('center_axis',(0.,1.,0.));
#6783=DIRECTION('ref_axis',(1.,0.,0.));
#6784=DIRECTION('center_axis',(0.,1.,0.));
#6785=DIRECTION('ref_axis',(1.,0.,0.));
#6786=DIRECTION('center_axis',(0.,1.,0.));
#6787=DIRECTION('ref_axis',(1.,0.,0.));
#6788=DIRECTION('',(0.,1.,0.));
#6789=DIRECTION('center_axis',(0.,1.,0.));
#6790=DIRECTION('ref_axis',(1.,0.,0.));
#6791=DIRECTION('center_axis',(0.,1.,0.));
#6792=DIRECTION('ref_axis',(1.,0.,0.));
#6793=DIRECTION('center_axis',(0.,1.,0.));
#6794=DIRECTION('ref_axis',(1.,0.,0.));
#6795=DIRECTION('center_axis',(0.,1.,0.));
#6796=DIRECTION('ref_axis',(1.,0.,0.));
#6797=DIRECTION('',(0.,1.,0.));
#6798=DIRECTION('center_axis',(0.,1.,0.));
#6799=DIRECTION('ref_axis',(1.,0.,0.));
#6800=DIRECTION('center_axis',(0.,1.,0.));
#6801=DIRECTION('ref_axis',(1.,0.,0.));
#6802=DIRECTION('center_axis',(0.,1.,0.));
#6803=DIRECTION('ref_axis',(1.,0.,0.));
#6804=DIRECTION('center_axis',(0.,1.,0.));
#6805=DIRECTION('ref_axis',(1.,0.,0.));
#6806=DIRECTION('',(0.,1.,0.));
#6807=DIRECTION('center_axis',(0.,1.,0.));
#6808=DIRECTION('ref_axis',(1.,0.,0.));
#6809=DIRECTION('center_axis',(0.,1.,0.));
#6810=DIRECTION('ref_axis',(1.,0.,0.));
#6811=DIRECTION('center_axis',(0.,1.,0.));
#6812=DIRECTION('ref_axis',(1.,0.,0.));
#6813=DIRECTION('center_axis',(0.,1.,0.));
#6814=DIRECTION('ref_axis',(1.,0.,0.));
#6815=DIRECTION('',(0.,1.,0.));
#6816=DIRECTION('center_axis',(0.,1.,0.));
#6817=DIRECTION('ref_axis',(1.,0.,0.));
#6818=DIRECTION('center_axis',(0.,1.,0.));
#6819=DIRECTION('ref_axis',(1.,0.,0.));
#6820=DIRECTION('center_axis',(0.,0.,1.));
#6821=DIRECTION('ref_axis',(1.,0.,0.));
#6822=DIRECTION('center_axis',(0.,0.,1.));
#6823=DIRECTION('ref_axis',(1.,0.,0.));
#6824=DIRECTION('',(0.,0.,1.));
#6825=DIRECTION('center_axis',(0.,0.,-1.));
#6826=DIRECTION('ref_axis',(1.,0.,0.));
#6827=DIRECTION('center_axis',(0.,0.,1.));
#6828=DIRECTION('ref_axis',(1.,0.,0.));
#6829=DIRECTION('center_axis',(0.,0.,1.));
#6830=DIRECTION('ref_axis',(1.,0.,0.));
#6831=DIRECTION('',(0.,0.,1.));
#6832=DIRECTION('center_axis',(0.,0.,-1.));
#6833=DIRECTION('ref_axis',(1.,0.,0.));
#6834=DIRECTION('center_axis',(0.,0.,1.));
#6835=DIRECTION('ref_axis',(1.,0.,0.));
#6836=DIRECTION('center_axis',(0.,0.,1.));
#6837=DIRECTION('ref_axis',(1.,0.,0.));
#6838=DIRECTION('',(0.,0.,1.));
#6839=DIRECTION('center_axis',(0.,0.,-1.));
#6840=DIRECTION('ref_axis',(1.,0.,0.));
#6841=DIRECTION('center_axis',(0.,0.,1.));
#6842=DIRECTION('ref_axis',(1.,0.,0.));
#6843=DIRECTION('center_axis',(0.,0.,1.));
#6844=DIRECTION('ref_axis',(1.,0.,0.));
#6845=DIRECTION('',(0.,0.,1.));
#6846=DIRECTION('center_axis',(0.,0.,-1.));
#6847=DIRECTION('ref_axis',(1.,0.,0.));
#6848=DIRECTION('center_axis',(0.,1.,0.));
#6849=DIRECTION('ref_axis',(0.,0.,1.));
#6850=DIRECTION('center_axis',(0.,1.,0.));
#6851=DIRECTION('ref_axis',(1.,0.,0.));
#6852=DIRECTION('',(1.,0.,0.));
#6853=DIRECTION('',(0.,0.,-1.));
#6854=DIRECTION('',(-1.,0.,0.));
#6855=DIRECTION('center_axis',(0.,1.,0.));
#6856=DIRECTION('ref_axis',(0.,0.,1.));
#6857=DIRECTION('center_axis',(0.,1.,0.));
#6858=DIRECTION('ref_axis',(1.,0.,0.));
#6859=DIRECTION('',(-1.,0.,0.));
#6860=DIRECTION('',(0.,0.,1.));
#6861=DIRECTION('',(1.,0.,0.));
#6862=DIRECTION('center_axis',(0.,1.,0.));
#6863=DIRECTION('ref_axis',(1.,0.,0.));
#6864=DIRECTION('center_axis',(0.,-1.,0.));
#6865=DIRECTION('ref_axis',(1.,0.,0.));
#6866=DIRECTION('',(1.,0.,0.));
#6867=DIRECTION('',(0.,0.,1.));
#6868=DIRECTION('',(-1.,0.,0.));
#6869=DIRECTION('center_axis',(0.,1.,0.));
#6870=DIRECTION('ref_axis',(1.,0.,0.));
#6871=DIRECTION('center_axis',(0.,-1.,0.));
#6872=DIRECTION('ref_axis',(1.,0.,0.));
#6873=DIRECTION('',(-1.,0.,0.));
#6874=DIRECTION('',(0.,0.,-1.));
#6875=DIRECTION('',(1.,0.,0.));
#6876=DIRECTION('center_axis',(0.,0.,1.));
#6877=DIRECTION('ref_axis',(1.,0.,0.));
#6878=DIRECTION('',(0.,1.,0.));
#6879=DIRECTION('',(0.,1.,0.));
#6880=DIRECTION('center_axis',(0.,0.,1.));
#6881=DIRECTION('ref_axis',(1.,0.,0.));
#6882=DIRECTION('',(0.,-1.,0.));
#6883=DIRECTION('',(0.,1.,0.));
#6884=DIRECTION('center_axis',(-1.,0.,0.));
#6885=DIRECTION('ref_axis',(0.,0.,1.));
#6886=DIRECTION('',(0.,1.,0.));
#6887=DIRECTION('center_axis',(0.,0.,-1.));
#6888=DIRECTION('ref_axis',(-1.,0.,0.));
#6889=DIRECTION('',(0.,1.,0.));
#6890=DIRECTION('center_axis',(1.,0.,0.));
#6891=DIRECTION('ref_axis',(0.,0.,-1.));
#6892=DIRECTION('center_axis',(0.,1.,0.));
#6893=DIRECTION('ref_axis',(0.,0.,1.));
#6894=DIRECTION('center_axis',(0.,1.,0.));
#6895=DIRECTION('ref_axis',(1.,0.,0.));
#6896=DIRECTION('',(1.,0.,0.));
#6897=DIRECTION('',(0.,0.,-1.));
#6898=DIRECTION('',(-1.,0.,0.));
#6899=DIRECTION('center_axis',(0.,1.,0.));
#6900=DIRECTION('ref_axis',(0.,0.,1.));
#6901=DIRECTION('center_axis',(0.,1.,0.));
#6902=DIRECTION('ref_axis',(1.,0.,0.));
#6903=DIRECTION('',(-1.,0.,0.));
#6904=DIRECTION('',(0.,0.,1.));
#6905=DIRECTION('',(1.,0.,0.));
#6906=DIRECTION('center_axis',(0.,1.,0.));
#6907=DIRECTION('ref_axis',(1.,0.,0.));
#6908=DIRECTION('center_axis',(0.,-1.,0.));
#6909=DIRECTION('ref_axis',(1.,0.,0.));
#6910=DIRECTION('',(1.,0.,0.));
#6911=DIRECTION('',(0.,0.,1.));
#6912=DIRECTION('',(-1.,0.,0.));
#6913=DIRECTION('center_axis',(0.,1.,0.));
#6914=DIRECTION('ref_axis',(1.,0.,0.));
#6915=DIRECTION('center_axis',(0.,-1.,0.));
#6916=DIRECTION('ref_axis',(1.,0.,0.));
#6917=DIRECTION('',(-1.,0.,0.));
#6918=DIRECTION('',(0.,0.,-1.));
#6919=DIRECTION('',(1.,0.,0.));
#6920=DIRECTION('center_axis',(0.,0.,1.));
#6921=DIRECTION('ref_axis',(1.,0.,0.));
#6922=DIRECTION('',(0.,1.,0.));
#6923=DIRECTION('',(0.,1.,0.));
#6924=DIRECTION('center_axis',(0.,0.,1.));
#6925=DIRECTION('ref_axis',(1.,0.,0.));
#6926=DIRECTION('',(0.,-1.,0.));
#6927=DIRECTION('',(0.,1.,0.));
#6928=DIRECTION('center_axis',(-1.,0.,0.));
#6929=DIRECTION('ref_axis',(0.,0.,1.));
#6930=DIRECTION('',(0.,1.,0.));
#6931=DIRECTION('center_axis',(0.,0.,-1.));
#6932=DIRECTION('ref_axis',(-1.,0.,0.));
#6933=DIRECTION('',(0.,1.,0.));
#6934=DIRECTION('center_axis',(1.,0.,0.));
#6935=DIRECTION('ref_axis',(0.,0.,-1.));
#6936=DIRECTION('center_axis',(0.,1.,0.));
#6937=DIRECTION('ref_axis',(1.,0.,0.));
#6938=DIRECTION('center_axis',(0.,-1.,0.));
#6939=DIRECTION('ref_axis',(1.,0.,0.));
#6940=DIRECTION('',(0.,-1.,0.));
#6941=DIRECTION('center_axis',(0.,-1.,0.));
#6942=DIRECTION('ref_axis',(1.,0.,0.));
#6943=DIRECTION('center_axis',(0.,1.,0.));
#6944=DIRECTION('ref_axis',(1.,0.,0.));
#6945=DIRECTION('center_axis',(0.,1.,0.));
#6946=DIRECTION('ref_axis',(1.,0.,0.));
#6947=DIRECTION('',(0.,-1.,0.));
#6948=DIRECTION('center_axis',(0.,1.,0.));
#6949=DIRECTION('ref_axis',(1.,0.,0.));
#6950=DIRECTION('center_axis',(0.,1.,0.));
#6951=DIRECTION('ref_axis',(1.,0.,0.));
#6952=DIRECTION('center_axis',(0.,1.,0.));
#6953=DIRECTION('ref_axis',(1.,0.,0.));
#6954=DIRECTION('axis',(0.,0.,1.));
#6955=DIRECTION('refdir',(1.,0.,0.));
#6956=DIRECTION('center_axis',(0.,1.,0.));
#6957=DIRECTION('ref_axis',(1.,0.,0.));
#6958=DIRECTION('center_axis',(0.,-1.,0.));
#6959=DIRECTION('ref_axis',(1.,0.,0.));
#6960=DIRECTION('',(0.,-1.,0.));
#6961=DIRECTION('center_axis',(0.,-1.,0.));
#6962=DIRECTION('ref_axis',(1.,0.,0.));
#6963=DIRECTION('center_axis',(0.,1.,0.));
#6964=DIRECTION('ref_axis',(1.,0.,0.));
#6965=DIRECTION('center_axis',(0.,1.,0.));
#6966=DIRECTION('ref_axis',(1.,0.,0.));
#6967=DIRECTION('',(0.,-1.,0.));
#6968=DIRECTION('center_axis',(0.,1.,0.));
#6969=DIRECTION('ref_axis',(1.,0.,0.));
#6970=DIRECTION('center_axis',(0.,1.,0.));
#6971=DIRECTION('ref_axis',(1.,0.,0.));
#6972=DIRECTION('center_axis',(0.,1.,0.));
#6973=DIRECTION('ref_axis',(1.,0.,0.));
#6974=DIRECTION('axis',(0.,0.,1.));
#6975=DIRECTION('refdir',(1.,0.,0.));
#6976=DIRECTION('center_axis',(0.,1.,0.));
#6977=DIRECTION('ref_axis',(1.,0.,0.));
#6978=DIRECTION('center_axis',(0.,1.,0.));
#6979=DIRECTION('ref_axis',(1.,0.,0.));
#6980=DIRECTION('',(0.,1.,0.));
#6981=DIRECTION('center_axis',(0.,-1.,0.));
#6982=DIRECTION('ref_axis',(1.,0.,0.));
#6983=DIRECTION('center_axis',(0.,1.,0.));
#6984=DIRECTION('ref_axis',(1.,0.,0.));
#6985=DIRECTION('center_axis',(0.,1.,0.));
#6986=DIRECTION('ref_axis',(1.,0.,0.));
#6987=DIRECTION('',(0.,1.,0.));
#6988=DIRECTION('center_axis',(0.,-1.,0.));
#6989=DIRECTION('ref_axis',(1.,0.,0.));
#6990=DIRECTION('center_axis',(0.,1.,0.));
#6991=DIRECTION('ref_axis',(1.,0.,0.));
#6992=DIRECTION('center_axis',(0.,1.,0.));
#6993=DIRECTION('ref_axis',(1.,0.,0.));
#6994=DIRECTION('',(0.,1.,0.));
#6995=DIRECTION('center_axis',(0.,-1.,0.));
#6996=DIRECTION('ref_axis',(1.,0.,0.));
#6997=DIRECTION('center_axis',(0.,1.,0.));
#6998=DIRECTION('ref_axis',(1.,0.,0.));
#6999=DIRECTION('center_axis',(0.,1.,0.));
#7000=DIRECTION('ref_axis',(1.,0.,0.));
#7001=DIRECTION('',(0.,1.,0.));
#7002=DIRECTION('center_axis',(0.,-1.,0.));
#7003=DIRECTION('ref_axis',(1.,0.,0.));
#7004=DIRECTION('center_axis',(0.,1.,0.));
#7005=DIRECTION('ref_axis',(1.,0.,0.));
#7006=DIRECTION('center_axis',(0.,1.,0.));
#7007=DIRECTION('ref_axis',(1.,0.,0.));
#7008=DIRECTION('',(0.,-1.,0.));
#7009=DIRECTION('center_axis',(0.,-1.,0.));
#7010=DIRECTION('ref_axis',(1.,0.,0.));
#7011=DIRECTION('center_axis',(0.,1.,0.));
#7012=DIRECTION('ref_axis',(1.,0.,0.));
#7013=DIRECTION('center_axis',(0.,-1.,0.));
#7014=DIRECTION('ref_axis',(1.,0.,0.));
#7015=DIRECTION('center_axis',(0.,1.,0.));
#7016=DIRECTION('ref_axis',(1.,0.,0.));
#7017=DIRECTION('center_axis',(0.,1.,0.));
#7018=DIRECTION('ref_axis',(1.,0.,0.));
#7019=DIRECTION('',(0.,1.,0.));
#7020=DIRECTION('center_axis',(0.,1.,0.));
#7021=DIRECTION('ref_axis',(1.,0.,0.));
#7022=DIRECTION('center_axis',(0.,1.,0.));
#7023=DIRECTION('ref_axis',(1.,0.,0.));
#7024=DIRECTION('center_axis',(0.,-1.,0.));
#7025=DIRECTION('ref_axis',(1.,0.,0.));
#7026=DIRECTION('center_axis',(0.,1.,0.));
#7027=DIRECTION('ref_axis',(1.,0.,0.));
#7028=DIRECTION('',(0.,-1.,0.));
#7029=DIRECTION('center_axis',(0.,1.,0.));
#7030=DIRECTION('ref_axis',(1.,0.,0.));
#7031=DIRECTION('center_axis',(0.,1.,0.));
#7032=DIRECTION('ref_axis',(1.,0.,0.));
#7033=DIRECTION('',(0.,-1.,0.));
#7034=DIRECTION('center_axis',(0.,1.,0.));
#7035=DIRECTION('ref_axis',(1.,0.,0.));
#7036=DIRECTION('center_axis',(0.,1.,0.));
#7037=DIRECTION('ref_axis',(1.,0.,0.));
#7038=DIRECTION('center_axis',(0.,1.,0.));
#7039=DIRECTION('ref_axis',(1.,0.,0.));
#7040=DIRECTION('axis',(0.,0.,1.));
#7041=DIRECTION('refdir',(1.,0.,0.));
#7042=DIRECTION('center_axis',(0.,1.,0.));
#7043=DIRECTION('ref_axis',(1.,0.,0.));
#7044=DIRECTION('center_axis',(0.,-1.,0.));
#7045=DIRECTION('ref_axis',(1.,0.,0.));
#7046=DIRECTION('',(0.,-1.,0.));
#7047=DIRECTION('center_axis',(0.,-1.,0.));
#7048=DIRECTION('ref_axis',(1.,0.,0.));
#7049=DIRECTION('center_axis',(0.,1.,0.));
#7050=DIRECTION('ref_axis',(1.,0.,0.));
#7051=DIRECTION('center_axis',(0.,1.,0.));
#7052=DIRECTION('ref_axis',(1.,0.,0.));
#7053=DIRECTION('',(0.,-1.,0.));
#7054=DIRECTION('center_axis',(0.,1.,0.));
#7055=DIRECTION('ref_axis',(1.,0.,0.));
#7056=DIRECTION('center_axis',(0.,1.,0.));
#7057=DIRECTION('ref_axis',(1.,0.,0.));
#7058=DIRECTION('center_axis',(0.,1.,0.));
#7059=DIRECTION('ref_axis',(1.,0.,0.));
#7060=DIRECTION('axis',(0.,0.,1.));
#7061=DIRECTION('refdir',(1.,0.,0.));
#7062=DIRECTION('center_axis',(0.,1.,0.));
#7063=DIRECTION('ref_axis',(1.,0.,0.));
#7064=DIRECTION('center_axis',(0.,1.,0.));
#7065=DIRECTION('ref_axis',(1.,0.,0.));
#7066=DIRECTION('',(0.,1.,0.));
#7067=DIRECTION('center_axis',(0.,-1.,0.));
#7068=DIRECTION('ref_axis',(1.,0.,0.));
#7069=DIRECTION('center_axis',(0.,1.,0.));
#7070=DIRECTION('ref_axis',(1.,0.,0.));
#7071=DIRECTION('center_axis',(0.,1.,0.));
#7072=DIRECTION('ref_axis',(1.,0.,0.));
#7073=DIRECTION('',(0.,1.,0.));
#7074=DIRECTION('center_axis',(0.,-1.,0.));
#7075=DIRECTION('ref_axis',(1.,0.,0.));
#7076=DIRECTION('center_axis',(0.,1.,0.));
#7077=DIRECTION('ref_axis',(1.,0.,0.));
#7078=DIRECTION('center_axis',(0.,1.,0.));
#7079=DIRECTION('ref_axis',(1.,0.,0.));
#7080=DIRECTION('',(0.,1.,0.));
#7081=DIRECTION('center_axis',(0.,-1.,0.));
#7082=DIRECTION('ref_axis',(1.,0.,0.));
#7083=DIRECTION('center_axis',(0.,1.,0.));
#7084=DIRECTION('ref_axis',(1.,0.,0.));
#7085=DIRECTION('center_axis',(0.,1.,0.));
#7086=DIRECTION('ref_axis',(1.,0.,0.));
#7087=DIRECTION('',(0.,1.,0.));
#7088=DIRECTION('center_axis',(0.,-1.,0.));
#7089=DIRECTION('ref_axis',(1.,0.,0.));
#7090=DIRECTION('center_axis',(0.,1.,0.));
#7091=DIRECTION('ref_axis',(1.,0.,0.));
#7092=DIRECTION('center_axis',(0.,1.,0.));
#7093=DIRECTION('ref_axis',(1.,0.,0.));
#7094=DIRECTION('',(0.,-1.,0.));
#7095=DIRECTION('center_axis',(0.,1.,0.));
#7096=DIRECTION('ref_axis',(1.,0.,0.));
#7097=DIRECTION('center_axis',(0.,1.,0.));
#7098=DIRECTION('ref_axis',(1.,0.,0.));
#7099=DIRECTION('center_axis',(0.,-1.,0.));
#7100=DIRECTION('ref_axis',(1.,0.,0.));
#7101=DIRECTION('center_axis',(0.,1.,0.));
#7102=DIRECTION('ref_axis',(1.,0.,0.));
#7103=DIRECTION('center_axis',(0.,-1.,0.));
#7104=DIRECTION('ref_axis',(1.,0.,0.));
#7105=DIRECTION('',(0.,-1.,0.));
#7106=DIRECTION('center_axis',(0.,1.,0.));
#7107=DIRECTION('ref_axis',(1.,0.,0.));
#7108=DIRECTION('center_axis',(0.,1.,0.));
#7109=DIRECTION('ref_axis',(1.,0.,0.));
#7110=DIRECTION('',(0.,-1.,0.));
#7111=DIRECTION('center_axis',(0.,1.,0.));
#7112=DIRECTION('ref_axis',(1.,0.,0.));
#7113=DIRECTION('center_axis',(0.,1.,0.));
#7114=DIRECTION('ref_axis',(1.,0.,0.));
#7115=DIRECTION('center_axis',(0.,1.,0.));
#7116=DIRECTION('ref_axis',(1.,0.,0.));
#7117=DIRECTION('axis',(0.,0.,1.));
#7118=DIRECTION('refdir',(1.,0.,0.));
#7119=DIRECTION('center_axis',(0.,1.,0.));
#7120=DIRECTION('ref_axis',(-1.,0.,0.));
#7121=DIRECTION('',(-1.,0.,0.));
#7122=DIRECTION('',(0.,0.,1.));
#7123=DIRECTION('',(-1.,0.,0.));
#7124=DIRECTION('',(0.,0.,1.));
#7125=DIRECTION('center_axis',(1.,0.,0.));
#7126=DIRECTION('ref_axis',(0.,1.,0.));
#7127=DIRECTION('',(0.,1.,0.));
#7128=DIRECTION('',(0.,1.,0.));
#7129=DIRECTION('',(0.,0.,1.));
#7130=DIRECTION('center_axis',(0.,-1.,0.));
#7131=DIRECTION('ref_axis',(1.,0.,0.));
#7132=DIRECTION('',(1.,0.,0.));
#7133=DIRECTION('',(1.,0.,0.));
#7134=DIRECTION('',(0.,0.,1.));
#7135=DIRECTION('center_axis',(-1.,0.,0.));
#7136=DIRECTION('ref_axis',(0.,-1.,0.));
#7137=DIRECTION('',(0.,-1.,0.));
#7138=DIRECTION('',(0.,-1.,0.));
#7139=DIRECTION('center_axis',(0.,0.,1.));
#7140=DIRECTION('ref_axis',(1.,0.,0.));
#7141=DIRECTION('center_axis',(0.,0.,1.));
#7142=DIRECTION('ref_axis',(1.,0.,0.));
#7143=DIRECTION('axis',(0.,0.,1.));
#7144=DIRECTION('refdir',(1.,0.,0.));
#7145=DIRECTION('center_axis',(0.,1.,0.));
#7146=DIRECTION('ref_axis',(-1.,0.,0.));
#7147=DIRECTION('',(-1.,0.,0.));
#7148=DIRECTION('',(0.,0.,1.));
#7149=DIRECTION('',(-1.,0.,0.));
#7150=DIRECTION('',(0.,0.,1.));
#7151=DIRECTION('center_axis',(1.,0.,0.));
#7152=DIRECTION('ref_axis',(0.,1.,0.));
#7153=DIRECTION('',(0.,1.,0.));
#7154=DIRECTION('',(0.,1.,0.));
#7155=DIRECTION('',(0.,0.,1.));
#7156=DIRECTION('center_axis',(0.,-1.,0.));
#7157=DIRECTION('ref_axis',(1.,0.,0.));
#7158=DIRECTION('',(1.,0.,0.));
#7159=DIRECTION('',(1.,0.,0.));
#7160=DIRECTION('',(0.,0.,1.));
#7161=DIRECTION('center_axis',(-1.,0.,0.));
#7162=DIRECTION('ref_axis',(0.,-1.,0.));
#7163=DIRECTION('',(0.,-1.,0.));
#7164=DIRECTION('',(0.,-1.,0.));
#7165=DIRECTION('center_axis',(0.,0.,1.));
#7166=DIRECTION('ref_axis',(1.,0.,0.));
#7167=DIRECTION('center_axis',(0.,0.,1.));
#7168=DIRECTION('ref_axis',(1.,0.,0.));
#7169=DIRECTION('axis',(0.,0.,1.));
#7170=DIRECTION('refdir',(1.,0.,0.));
#7171=DIRECTION('axis',(0.,0.,1.));
#7172=DIRECTION('refdir',(1.,0.,0.));
#7173=DIRECTION('center_axis',(0.,-1.,0.));
#7174=DIRECTION('ref_axis',(0.,0.,-1.));
#7175=DIRECTION('center_axis',(0.,-1.,0.));
#7176=DIRECTION('ref_axis',(1.,0.,0.));
#7177=DIRECTION('center_axis',(0.,-1.,0.));
#7178=DIRECTION('ref_axis',(1.,0.,0.));
#7179=DIRECTION('center_axis',(1.,0.,1.22464679914735E-16));
#7180=DIRECTION('ref_axis',(-1.22464679914735E-16,0.,1.));
#7181=DIRECTION('center_axis',(0.,1.,0.));
#7182=DIRECTION('ref_axis',(1.,0.,0.));
#7183=DIRECTION('center_axis',(0.,1.,0.));
#7184=DIRECTION('ref_axis',(1.,0.,0.));
#7185=DIRECTION('center_axis',(0.,-1.,0.));
#7186=DIRECTION('ref_axis',(1.,0.,0.));
#7187=DIRECTION('',(0.,1.,0.));
#7188=DIRECTION('center_axis',(0.,-1.,0.));
#7189=DIRECTION('ref_axis',(1.,0.,0.));
#7190=DIRECTION('center_axis',(0.,-1.,0.));
#7191=DIRECTION('ref_axis',(1.,0.,0.));
#7192=DIRECTION('center_axis',(0.,-1.,0.));
#7193=DIRECTION('ref_axis',(1.,0.,0.));
#7194=DIRECTION('',(0.,1.,0.));
#7195=DIRECTION('center_axis',(0.,-1.,0.));
#7196=DIRECTION('ref_axis',(1.,0.,0.));
#7197=DIRECTION('center_axis',(0.,1.,0.));
#7198=DIRECTION('ref_axis',(1.,0.,0.));
#7199=DIRECTION('',(-0.707106781186548,0.707106781186547,-8.65956056235494E-17));
#7200=DIRECTION('center_axis',(0.,-1.,0.));
#7201=DIRECTION('ref_axis',(1.,0.,0.));
#7202=DIRECTION('center_axis',(0.,1.,0.));
#7203=DIRECTION('ref_axis',(0.,0.,1.));
#7204=DIRECTION('center_axis',(0.,-1.,0.));
#7205=DIRECTION('ref_axis',(1.,0.,0.));
#7206=DIRECTION('center_axis',(0.,-1.,0.));
#7207=DIRECTION('ref_axis',(1.,0.,0.));
#7208=DIRECTION('',(0.,1.,0.));
#7209=DIRECTION('center_axis',(0.,-1.,0.));
#7210=DIRECTION('ref_axis',(0.,0.,-1.));
#7211=DIRECTION('center_axis',(0.,-1.,0.));
#7212=DIRECTION('ref_axis',(1.,0.,0.));
#7213=DIRECTION('center_axis',(0.,-1.,0.));
#7214=DIRECTION('ref_axis',(1.,0.,0.));
#7215=DIRECTION('',(0.707106781186548,0.707106781186547,8.65956056235494E-17));
#7216=DIRECTION('axis',(0.,0.,1.));
#7217=DIRECTION('refdir',(1.,0.,0.));
#7218=DIRECTION('center_axis',(0.,-1.,0.));
#7219=DIRECTION('ref_axis',(0.,0.,-1.));
#7220=DIRECTION('center_axis',(0.,-1.,0.));
#7221=DIRECTION('ref_axis',(1.,0.,0.));
#7222=DIRECTION('center_axis',(0.,-1.,0.));
#7223=DIRECTION('ref_axis',(1.,0.,0.));
#7224=DIRECTION('center_axis',(1.,0.,1.22464679914735E-16));
#7225=DIRECTION('ref_axis',(-1.22464679914735E-16,0.,1.));
#7226=DIRECTION('center_axis',(0.,1.,0.));
#7227=DIRECTION('ref_axis',(1.,0.,0.));
#7228=DIRECTION('center_axis',(0.,1.,0.));
#7229=DIRECTION('ref_axis',(1.,0.,0.));
#7230=DIRECTION('center_axis',(0.,-1.,0.));
#7231=DIRECTION('ref_axis',(1.,0.,0.));
#7232=DIRECTION('center_axis',(0.,-1.,0.));
#7233=DIRECTION('ref_axis',(1.,0.,0.));
#7234=DIRECTION('',(0.,1.,0.));
#7235=DIRECTION('center_axis',(0.,1.,0.));
#7236=DIRECTION('ref_axis',(0.,0.,1.));
#7237=DIRECTION('center_axis',(0.,-1.,0.));
#7238=DIRECTION('ref_axis',(1.,0.,0.));
#7239=DIRECTION('center_axis',(0.,-1.,0.));
#7240=DIRECTION('ref_axis',(1.,0.,0.));
#7241=DIRECTION('center_axis',(0.,-1.,0.));
#7242=DIRECTION('ref_axis',(1.,0.,0.));
#7243=DIRECTION('center_axis',(0.,-1.,0.));
#7244=DIRECTION('ref_axis',(1.,0.,0.));
#7245=DIRECTION('',(0.707106781186548,0.707106781186547,8.65956056235494E-17));
#7246=DIRECTION('center_axis',(0.,-1.,0.));
#7247=DIRECTION('ref_axis',(1.,0.,0.));
#7248=DIRECTION('center_axis',(0.,-1.,0.));
#7249=DIRECTION('ref_axis',(1.,0.,0.));
#7250=DIRECTION('',(0.,1.,0.));
#7251=DIRECTION('center_axis',(0.,1.,0.));
#7252=DIRECTION('ref_axis',(1.,0.,0.));
#7253=DIRECTION('center_axis',(0.,-1.,0.));
#7254=DIRECTION('ref_axis',(1.,0.,0.));
#7255=DIRECTION('',(-0.707106781186548,0.707106781186547,-8.65956056235494E-17));
#7256=DIRECTION('center_axis',(0.,-1.,0.));
#7257=DIRECTION('ref_axis',(0.,0.,-1.));
#7258=DIRECTION('center_axis',(0.,-1.,0.));
#7259=DIRECTION('ref_axis',(1.,0.,0.));
#7260=DIRECTION('',(0.,1.,0.));
#7261=DIRECTION('axis',(0.,0.,1.));
#7262=DIRECTION('refdir',(1.,0.,0.));
#7263=DIRECTION('center_axis',(0.,0.,1.));
#7264=DIRECTION('ref_axis',(1.,0.,0.));
#7265=DIRECTION('center_axis',(1.22464679914735E-16,-1.,0.));
#7266=DIRECTION('ref_axis',(-1.,-1.22464679914735E-16,0.));
#7267=DIRECTION('center_axis',(0.707106781186548,0.,0.707106781186548));
#7268=DIRECTION('ref_axis',(0.707106781186548,0.,-0.707106781186548));
#7269=DIRECTION('center_axis',(8.65956056235493E-17,-1.,-8.65956056235493E-17));
#7270=DIRECTION('ref_axis',(-0.707106781186548,-1.22464679914735E-16,0.707106781186548));
#7271=DIRECTION('center_axis',(1.,0.,0.));
#7272=DIRECTION('ref_axis',(6.12323399573677E-17,0.,-1.));
#7273=DIRECTION('center_axis',(7.49879891330929E-33,-1.,-1.22464679914735E-16));
#7274=DIRECTION('ref_axis',(-6.12323399573677E-17,-1.22464679914735E-16,
1.));
#7275=DIRECTION('center_axis',(0.707106781186548,0.,-0.707106781186548));
#7276=DIRECTION('ref_axis',(-0.707106781186548,0.,-0.707106781186548));
#7277=DIRECTION('center_axis',(-8.65956056235493E-17,-1.,-8.65956056235493E-17));
#7278=DIRECTION('ref_axis',(0.707106781186548,-1.22464679914735E-16,0.707106781186548));
#7279=DIRECTION('center_axis',(0.,0.,-1.));
#7280=DIRECTION('ref_axis',(-1.,0.,-1.22464679914735E-16));
#7281=DIRECTION('center_axis',(-1.22464679914735E-16,-1.,-1.49975978266186E-32));
#7282=DIRECTION('ref_axis',(1.,-1.22464679914735E-16,1.22464679914735E-16));
#7283=DIRECTION('center_axis',(-0.707106781186548,0.,-0.707106781186548));
#7284=DIRECTION('ref_axis',(-0.707106781186548,0.,0.707106781186548));
#7285=DIRECTION('center_axis',(-8.65956056235493E-17,-1.,8.65956056235493E-17));
#7286=DIRECTION('ref_axis',(0.707106781186548,-1.22464679914735E-16,-0.707106781186548));
#7287=DIRECTION('center_axis',(-1.,0.,0.));
#7288=DIRECTION('ref_axis',(-1.83697019872103E-16,0.,1.));
#7289=DIRECTION('center_axis',(-2.24963967399279E-32,-1.,1.22464679914735E-16));
#7290=DIRECTION('ref_axis',(1.83697019872103E-16,-1.22464679914735E-16,
-1.));
#7291=DIRECTION('center_axis',(-0.707106781186548,0.,0.707106781186548));
#7292=DIRECTION('ref_axis',(0.707106781186548,0.,0.707106781186548));
#7293=DIRECTION('center_axis',(8.65956056235493E-17,-1.,8.65956056235494E-17));
#7294=DIRECTION('ref_axis',(-0.707106781186548,-1.22464679914735E-16,-0.707106781186548));
#7295=DIRECTION('axis',(0.,0.,1.));
#7296=DIRECTION('refdir',(1.,0.,0.));
#7297=DIRECTION('center_axis',(0.,0.,1.));
#7298=DIRECTION('ref_axis',(1.,0.,0.));
#7299=DIRECTION('center_axis',(0.,-1.,0.));
#7300=DIRECTION('ref_axis',(0.,0.,-1.));
#7301=DIRECTION('center_axis',(0.,-1.,0.));
#7302=DIRECTION('ref_axis',(0.,0.,-1.));
#7303=DIRECTION('center_axis',(0.,1.,0.));
#7304=DIRECTION('ref_axis',(1.,0.,0.));
#7305=DIRECTION('center_axis',(0.,1.,0.));
#7306=DIRECTION('ref_axis',(1.,0.,0.));
#7307=DIRECTION('center_axis',(0.,1.,0.));
#7308=DIRECTION('ref_axis',(1.,0.,0.));
#7309=DIRECTION('center_axis',(0.,1.,0.));
#7310=DIRECTION('ref_axis',(1.,0.,0.));
#7311=DIRECTION('',(0.,-1.,0.));
#7312=DIRECTION('center_axis',(0.,-1.,0.));
#7313=DIRECTION('ref_axis',(1.,0.,0.));
#7314=DIRECTION('center_axis',(0.,1.,0.));
#7315=DIRECTION('ref_axis',(1.,0.,0.));
#7316=DIRECTION('center_axis',(0.,1.,0.));
#7317=DIRECTION('ref_axis',(1.,0.,0.));
#7318=DIRECTION('center_axis',(0.,1.,0.));
#7319=DIRECTION('ref_axis',(1.,0.,0.));
#7320=DIRECTION('center_axis',(0.,1.,0.));
#7321=DIRECTION('ref_axis',(1.,0.,0.));
#7322=DIRECTION('center_axis',(0.,1.,0.));
#7323=DIRECTION('ref_axis',(1.,0.,0.));
#7324=DIRECTION('center_axis',(0.,1.,0.));
#7325=DIRECTION('ref_axis',(1.,0.,0.));
#7326=DIRECTION('center_axis',(0.,-1.,0.));
#7327=DIRECTION('ref_axis',(1.,0.,0.));
#7328=DIRECTION('center_axis',(0.,-1.,0.));
#7329=DIRECTION('ref_axis',(0.,0.,-1.));
#7330=DIRECTION('center_axis',(6.12323399573677E-17,0.,1.));
#7331=DIRECTION('ref_axis',(1.,0.,0.));
#7332=DIRECTION('center_axis',(0.,-1.,0.));
#7333=DIRECTION('ref_axis',(0.,0.,-1.));
#7334=DIRECTION('center_axis',(0.,1.,0.));
#7335=DIRECTION('ref_axis',(1.,0.,0.));
#7336=DIRECTION('center_axis',(0.,-1.,0.));
#7337=DIRECTION('ref_axis',(1.,0.,0.));
#7338=DIRECTION('center_axis',(0.,-1.,0.));
#7339=DIRECTION('ref_axis',(0.,0.,-1.));
#7340=DIRECTION('center_axis',(0.,0.,1.));
#7341=DIRECTION('ref_axis',(1.,0.,0.));
#7342=DIRECTION('center_axis',(0.,-1.,0.));
#7343=DIRECTION('ref_axis',(0.,0.,-1.));
#7344=DIRECTION('center_axis',(0.,1.,0.));
#7345=DIRECTION('ref_axis',(1.,0.,0.));
#7346=DIRECTION('center_axis',(0.,-1.,0.));
#7347=DIRECTION('ref_axis',(1.,0.,0.));
#7348=DIRECTION('center_axis',(0.,-1.,0.));
#7349=DIRECTION('ref_axis',(0.,0.,-1.));
#7350=DIRECTION('center_axis',(0.,0.,1.));
#7351=DIRECTION('ref_axis',(1.,0.,0.));
#7352=DIRECTION('center_axis',(0.,-1.,0.));
#7353=DIRECTION('ref_axis',(0.,0.,-1.));
#7354=DIRECTION('center_axis',(0.,1.,0.));
#7355=DIRECTION('ref_axis',(1.,0.,0.));
#7356=DIRECTION('center_axis',(0.,-1.,0.));
#7357=DIRECTION('ref_axis',(1.,0.,0.));
#7358=DIRECTION('center_axis',(0.,-1.,0.));
#7359=DIRECTION('ref_axis',(0.,0.,-1.));
#7360=DIRECTION('center_axis',(0.,0.,1.));
#7361=DIRECTION('ref_axis',(1.,0.,0.));
#7362=DIRECTION('center_axis',(0.,-1.,0.));
#7363=DIRECTION('ref_axis',(0.,0.,-1.));
#7364=DIRECTION('center_axis',(0.,1.,0.));
#7365=DIRECTION('ref_axis',(1.,0.,0.));
#7366=DIRECTION('center_axis',(0.,-1.,0.));
#7367=DIRECTION('ref_axis',(1.,0.,0.));
#7368=DIRECTION('center_axis',(0.,-1.,0.));
#7369=DIRECTION('ref_axis',(0.,0.,-1.));
#7370=DIRECTION('center_axis',(6.12323399573676E-17,0.,1.));
#7371=DIRECTION('ref_axis',(1.,0.,0.));
#7372=DIRECTION('center_axis',(0.,-1.,0.));
#7373=DIRECTION('ref_axis',(0.,0.,-1.));
#7374=DIRECTION('center_axis',(0.,1.,0.));
#7375=DIRECTION('ref_axis',(1.,0.,0.));
#7376=DIRECTION('center_axis',(0.,-1.,0.));
#7377=DIRECTION('ref_axis',(1.,0.,0.));
#7378=DIRECTION('center_axis',(0.,-1.,0.));
#7379=DIRECTION('ref_axis',(0.,0.,-1.));
#7380=DIRECTION('center_axis',(0.,0.,1.));
#7381=DIRECTION('ref_axis',(1.,0.,0.));
#7382=DIRECTION('center_axis',(0.,-1.,0.));
#7383=DIRECTION('ref_axis',(0.,0.,-1.));
#7384=DIRECTION('center_axis',(0.,1.,0.));
#7385=DIRECTION('ref_axis',(1.,0.,0.));
#7386=DIRECTION('center_axis',(0.,1.,0.));
#7387=DIRECTION('ref_axis',(1.,0.,0.));
#7388=DIRECTION('',(0.,1.,0.));
#7389=DIRECTION('center_axis',(0.,-1.,0.));
#7390=DIRECTION('ref_axis',(1.,0.,0.));
#7391=DIRECTION('center_axis',(0.,-1.,0.));
#7392=DIRECTION('ref_axis',(1.,0.,0.));
#7393=DIRECTION('center_axis',(0.,1.,0.));
#7394=DIRECTION('ref_axis',(1.,0.,0.));
#7395=DIRECTION('center_axis',(0.,-1.,0.));
#7396=DIRECTION('ref_axis',(0.,0.,-1.));
#7397=DIRECTION('center_axis',(0.,0.,1.));
#7398=DIRECTION('ref_axis',(1.,0.,0.));
#7399=DIRECTION('center_axis',(0.,-1.,0.));
#7400=DIRECTION('ref_axis',(0.,0.,-1.));
#7401=DIRECTION('center_axis',(0.,-1.,0.));
#7402=DIRECTION('ref_axis',(-1.,0.,0.));
#7403=DIRECTION('center_axis',(0.,1.,0.));
#7404=DIRECTION('ref_axis',(1.,0.,0.));
#7405=DIRECTION('axis',(0.,0.,1.));
#7406=DIRECTION('refdir',(1.,0.,0.));
#7407=DIRECTION('center_axis',(0.,1.,0.));
#7408=DIRECTION('ref_axis',(0.,0.,1.));
#7409=DIRECTION('center_axis',(0.,-1.,0.));
#7410=DIRECTION('ref_axis',(1.,0.,0.));
#7411=DIRECTION('center_axis',(0.,-1.,0.));
#7412=DIRECTION('ref_axis',(1.,0.,0.));
#7413=DIRECTION('center_axis',(0.,-1.,0.));
#7414=DIRECTION('ref_axis',(1.,0.,0.));
#7415=DIRECTION('center_axis',(0.,-1.,0.));
#7416=DIRECTION('ref_axis',(1.,0.,0.));
#7417=DIRECTION('',(0.,1.,0.));
#7418=DIRECTION('center_axis',(0.,-1.,0.));
#7419=DIRECTION('ref_axis',(0.,0.,-1.));
#7420=DIRECTION('center_axis',(0.,-1.,0.));
#7421=DIRECTION('ref_axis',(1.,0.,0.));
#7422=DIRECTION('center_axis',(0.,-1.,0.));
#7423=DIRECTION('ref_axis',(1.,0.,0.));
#7424=DIRECTION('',(0.,1.,0.));
#7425=DIRECTION('center_axis',(0.,1.,0.));
#7426=DIRECTION('ref_axis',(0.,0.,1.));
#7427=DIRECTION('center_axis',(0.,-1.,0.));
#7428=DIRECTION('ref_axis',(1.,0.,0.));
#7429=DIRECTION('center_axis',(0.,-1.,0.));
#7430=DIRECTION('ref_axis',(1.,0.,0.));
#7431=DIRECTION('center_axis',(0.,-1.,0.));
#7432=DIRECTION('ref_axis',(1.,0.,0.));
#7433=DIRECTION('center_axis',(0.,-1.,0.));
#7434=DIRECTION('ref_axis',(1.,0.,0.));
#7435=DIRECTION('',(0.,1.,0.));
#7436=DIRECTION('center_axis',(0.,-1.,0.));
#7437=DIRECTION('ref_axis',(0.,0.,-1.));
#7438=DIRECTION('center_axis',(0.,-1.,0.));
#7439=DIRECTION('ref_axis',(1.,0.,0.));
#7440=DIRECTION('center_axis',(0.,-1.,0.));
#7441=DIRECTION('ref_axis',(1.,0.,0.));
#7442=DIRECTION('',(0.,1.,0.));
#7443=DIRECTION('',(0.,0.,1.));
#7444=DIRECTION('',(1.,0.,0.));
#7445=DIRECTION('',(0.,0.,1.));
#7446=DIRECTION('',(1.,0.,0.));
#7447=DIRECTION('',(0.,0.,1.));
#7448=DIRECTION('',(1.,0.,0.));
#7449=DIRECTION('',(0.,0.,1.));
#7450=DIRECTION('',(1.,0.,0.));
#7451=DIRECTION('',(0.,0.,1.));
#7452=DIRECTION('',(1.,0.,0.));
#7453=DIRECTION('axis',(0.,0.,1.));
#7454=DIRECTION('refdir',(1.,0.,0.));
#7455=DIRECTION('center_axis',(0.,1.,0.));
#7456=DIRECTION('ref_axis',(0.,0.,1.));
#7457=DIRECTION('center_axis',(0.,-1.,0.));
#7458=DIRECTION('ref_axis',(1.,0.,0.));
#7459=DIRECTION('center_axis',(0.,-1.,0.));
#7460=DIRECTION('ref_axis',(1.,0.,0.));
#7461=DIRECTION('center_axis',(0.,-1.,0.));
#7462=DIRECTION('ref_axis',(1.,0.,0.));
#7463=DIRECTION('',(0.707106781186548,0.707106781186547,8.65956056235494E-17));
#7464=DIRECTION('center_axis',(0.,-1.,0.));
#7465=DIRECTION('ref_axis',(1.,0.,0.));
#7466=DIRECTION('center_axis',(0.,-1.,0.));
#7467=DIRECTION('ref_axis',(1.,0.,0.));
#7468=DIRECTION('',(0.,1.,0.));
#7469=DIRECTION('center_axis',(0.,1.,0.));
#7470=DIRECTION('ref_axis',(1.,0.,0.));
#7471=DIRECTION('center_axis',(0.,-1.,0.));
#7472=DIRECTION('ref_axis',(1.,0.,0.));
#7473=DIRECTION('',(-0.707106781186547,0.707106781186548,-8.65956056235493E-17));
#7474=DIRECTION('center_axis',(0.,-1.,0.));
#7475=DIRECTION('ref_axis',(0.,0.,-1.));
#7476=DIRECTION('center_axis',(0.,-1.,0.));
#7477=DIRECTION('ref_axis',(1.,0.,0.));
#7478=DIRECTION('center_axis',(0.,1.,0.));
#7479=DIRECTION('ref_axis',(1.,0.,0.));
#7480=DIRECTION('center_axis',(0.,1.,0.));
#7481=DIRECTION('ref_axis',(1.,0.,0.));
#7482=DIRECTION('',(-0.447213595499958,0.894427190999916,-5.47678698264203E-17));
#7483=DIRECTION('center_axis',(0.,-1.,0.));
#7484=DIRECTION('ref_axis',(1.,0.,0.));
#7485=DIRECTION('center_axis',(0.,1.,0.));
#7486=DIRECTION('ref_axis',(1.,0.,0.));
#7487=DIRECTION('',(0.,1.,0.));
#7488=DIRECTION('center_axis',(0.,1.,0.));
#7489=DIRECTION('ref_axis',(1.,0.,0.));
#7490=DIRECTION('center_axis',(0.,-1.,0.));
#7491=DIRECTION('ref_axis',(1.,0.,0.));
#7492=DIRECTION('',(-0.707106781186547,0.707106781186548,-8.65956056235493E-17));
#7493=DIRECTION('center_axis',(0.,-1.,0.));
#7494=DIRECTION('ref_axis',(0.,0.,-1.));
#7495=DIRECTION('center_axis',(0.866025403784439,0.,-0.5));
#7496=DIRECTION('ref_axis',(0.5,0.,0.866025403784439));
#7497=DIRECTION('',(-0.5,0.,-0.866025403784439));
#7498=DIRECTION('',(0.,-1.,0.));
#7499=DIRECTION('',(0.5,0.,0.866025403784439));
#7500=DIRECTION('',(0.,-1.,0.));
#7501=DIRECTION('center_axis',(1.92296268638356E-16,0.,-1.));
#7502=DIRECTION('ref_axis',(1.,0.,1.92296268638356E-16));
#7503=DIRECTION('',(-1.,0.,-1.92296268638356E-16));
#7504=DIRECTION('',(0.,-1.,0.));
#7505=DIRECTION('',(1.,0.,1.92296268638356E-16));
#7506=DIRECTION('center_axis',(-0.866025403784439,0.,-0.5));
#7507=DIRECTION('ref_axis',(0.5,0.,-0.866025403784439));
#7508=DIRECTION('',(-0.5,0.,0.866025403784438));
#7509=DIRECTION('',(0.,-1.,0.));
#7510=DIRECTION('',(0.5,0.,-0.866025403784438));
#7511=DIRECTION('center_axis',(-0.866025403784439,0.,0.5));
#7512=DIRECTION('ref_axis',(-0.5,0.,-0.866025403784439));
#7513=DIRECTION('',(0.5,0.,0.866025403784439));
#7514=DIRECTION('',(0.,-1.,0.));
#7515=DIRECTION('',(-0.5,0.,-0.866025403784439));
#7516=DIRECTION('center_axis',(-1.92296268638356E-16,0.,1.));
#7517=DIRECTION('ref_axis',(-1.,0.,-1.92296268638356E-16));
#7518=DIRECTION('',(1.,0.,1.92296268638356E-16));
#7519=DIRECTION('',(0.,-1.,0.));
#7520=DIRECTION('',(-1.,0.,-1.92296268638356E-16));
#7521=DIRECTION('center_axis',(0.866025403784439,0.,0.5));
#7522=DIRECTION('ref_axis',(-0.5,0.,0.866025403784439));
#7523=DIRECTION('',(0.5,0.,-0.866025403784439));
#7524=DIRECTION('',(-0.5,0.,0.866025403784439));
#7525=DIRECTION('center_axis',(0.,1.,0.));
#7526=DIRECTION('ref_axis',(1.,0.,0.));
#7527=DIRECTION('center_axis',(0.,-1.,0.));
#7528=DIRECTION('ref_axis',(0.,0.,-1.));
#7529=DIRECTION('axis',(0.,0.,1.));
#7530=DIRECTION('refdir',(1.,0.,0.));
#7531=DIRECTION('center_axis',(0.,1.,0.));
#7532=DIRECTION('ref_axis',(0.,0.,1.));
#7533=DIRECTION('center_axis',(0.,-1.,0.));
#7534=DIRECTION('ref_axis',(1.,0.,0.));
#7535=DIRECTION('center_axis',(0.,-1.,0.));
#7536=DIRECTION('ref_axis',(1.,0.,0.));
#7537=DIRECTION('center_axis',(0.,-1.,0.));
#7538=DIRECTION('ref_axis',(1.,0.,0.));
#7539=DIRECTION('',(0.707106781186547,0.707106781186548,8.65956056235493E-17));
#7540=DIRECTION('center_axis',(0.,-1.,0.));
#7541=DIRECTION('ref_axis',(1.,0.,0.));
#7542=DIRECTION('center_axis',(0.,-1.,0.));
#7543=DIRECTION('ref_axis',(1.,0.,0.));
#7544=DIRECTION('',(0.,1.,0.));
#7545=DIRECTION('center_axis',(0.,1.,0.));
#7546=DIRECTION('ref_axis',(1.,0.,0.));
#7547=DIRECTION('center_axis',(0.,-1.,0.));
#7548=DIRECTION('ref_axis',(1.,0.,0.));
#7549=DIRECTION('',(-0.707106781186547,0.707106781186548,-8.65956056235493E-17));
#7550=DIRECTION('center_axis',(0.,-1.,0.));
#7551=DIRECTION('ref_axis',(0.,0.,-1.));
#7552=DIRECTION('center_axis',(0.,-1.,0.));
#7553=DIRECTION('ref_axis',(1.,0.,0.));
#7554=DIRECTION('center_axis',(0.,1.,0.));
#7555=DIRECTION('ref_axis',(1.,0.,0.));
#7556=DIRECTION('center_axis',(0.,1.,0.));
#7557=DIRECTION('ref_axis',(1.,0.,0.));
#7558=DIRECTION('',(-0.447213595499958,0.894427190999916,-5.47678698264203E-17));
#7559=DIRECTION('center_axis',(0.,-1.,0.));
#7560=DIRECTION('ref_axis',(1.,0.,0.));
#7561=DIRECTION('center_axis',(0.,1.,0.));
#7562=DIRECTION('ref_axis',(1.,0.,0.));
#7563=DIRECTION('',(0.,1.,0.));
#7564=DIRECTION('center_axis',(0.,1.,0.));
#7565=DIRECTION('ref_axis',(1.,0.,0.));
#7566=DIRECTION('center_axis',(0.,-1.,0.));
#7567=DIRECTION('ref_axis',(1.,0.,0.));
#7568=DIRECTION('',(-0.707106781186547,0.707106781186548,-8.65956056235493E-17));
#7569=DIRECTION('center_axis',(0.,-1.,0.));
#7570=DIRECTION('ref_axis',(0.,0.,-1.));
#7571=DIRECTION('center_axis',(0.866025403784439,0.,-0.5));
#7572=DIRECTION('ref_axis',(0.5,0.,0.866025403784439));
#7573=DIRECTION('',(-0.5,0.,-0.866025403784439));
#7574=DIRECTION('',(0.,-1.,0.));
#7575=DIRECTION('',(0.5,0.,0.866025403784439));
#7576=DIRECTION('',(0.,-1.,0.));
#7577=DIRECTION('center_axis',(1.60246890531964E-16,0.,-1.));
#7578=DIRECTION('ref_axis',(1.,0.,1.60246890531964E-16));
#7579=DIRECTION('',(-1.,0.,-1.60246890531964E-16));
#7580=DIRECTION('',(0.,-1.,0.));
#7581=DIRECTION('',(1.,0.,1.60246890531964E-16));
#7582=DIRECTION('center_axis',(-0.866025403784439,0.,-0.5));
#7583=DIRECTION('ref_axis',(0.5,0.,-0.866025403784439));
#7584=DIRECTION('',(-0.5,0.,0.866025403784439));
#7585=DIRECTION('',(0.,-1.,0.));
#7586=DIRECTION('',(0.5,0.,-0.866025403784439));
#7587=DIRECTION('center_axis',(-0.866025403784439,0.,0.5));
#7588=DIRECTION('ref_axis',(-0.5,0.,-0.866025403784439));
#7589=DIRECTION('',(0.5,0.,0.866025403784439));
#7590=DIRECTION('',(0.,-1.,0.));
#7591=DIRECTION('',(-0.5,0.,-0.866025403784439));
#7592=DIRECTION('center_axis',(-1.60246890531964E-16,0.,1.));
#7593=DIRECTION('ref_axis',(-1.,0.,-1.60246890531964E-16));
#7594=DIRECTION('',(1.,0.,1.60246890531964E-16));
#7595=DIRECTION('',(0.,-1.,0.));
#7596=DIRECTION('',(-1.,0.,-1.60246890531964E-16));
#7597=DIRECTION('center_axis',(0.866025403784439,0.,0.5));
#7598=DIRECTION('ref_axis',(-0.5,0.,0.866025403784439));
#7599=DIRECTION('',(0.5,0.,-0.866025403784439));
#7600=DIRECTION('',(-0.5,0.,0.866025403784439));
#7601=DIRECTION('center_axis',(0.,1.,0.));
#7602=DIRECTION('ref_axis',(1.,0.,0.));
#7603=DIRECTION('center_axis',(0.,-1.,0.));
#7604=DIRECTION('ref_axis',(0.,0.,-1.));
#7605=DIRECTION('',(0.,0.,1.));
#7606=DIRECTION('',(1.,0.,0.));
#7607=DIRECTION('',(0.,0.,1.));
#7608=DIRECTION('',(1.,0.,0.));
#7609=DIRECTION('',(0.,0.,1.));
#7610=DIRECTION('',(1.,0.,0.));
#7611=DIRECTION('',(0.,0.,1.));
#7612=DIRECTION('',(1.,0.,0.));
#7613=DIRECTION('',(0.,0.,1.));
#7614=DIRECTION('',(1.,0.,0.));
#7615=DIRECTION('',(0.,0.,1.));
#7616=DIRECTION('',(1.,0.,0.));
#7617=DIRECTION('',(0.,0.,1.));
#7618=DIRECTION('',(1.,0.,0.));
#7619=DIRECTION('',(0.,0.,1.));
#7620=DIRECTION('',(1.,0.,0.));
#7621=DIRECTION('',(0.,0.,1.));
#7622=DIRECTION('',(1.,0.,0.));
#7623=DIRECTION('',(0.,-1.,2.22044604925031E-16));
#7624=DIRECTION('',(1.,0.,0.));
#7625=DIRECTION('',(0.,-1.,2.22044604925031E-16));
#7626=DIRECTION('',(1.,0.,0.));
#7627=DIRECTION('',(0.,0.,1.));
#7628=DIRECTION('',(1.,0.,0.));
#7629=DIRECTION('',(0.,-1.,2.22044604925031E-16));
#7630=DIRECTION('',(1.,0.,0.));
#7631=DIRECTION('',(0.,-1.,2.22044604925031E-16));
#7632=DIRECTION('',(1.,0.,0.));
#7633=DIRECTION('',(0.,0.,1.));
#7634=DIRECTION('',(-1.,1.22464679914735E-16,0.));
#7635=DIRECTION('',(0.,0.,1.));
#7636=DIRECTION('',(-1.,1.22464679914735E-16,0.));
#7637=DIRECTION('',(0.,0.,1.));
#7638=DIRECTION('',(-1.,1.22464679914735E-16,0.));
#7639=DIRECTION('',(0.,0.,1.));
#7640=DIRECTION('',(-1.,1.22464679914735E-16,0.));
#7641=DIRECTION('',(0.,0.,1.));
#7642=DIRECTION('',(1.,0.,0.));
#7643=DIRECTION('',(0.,0.,1.));
#7644=DIRECTION('',(1.,0.,0.));
#7645=DIRECTION('',(0.,0.,1.));
#7646=DIRECTION('',(1.,0.,0.));
#7647=DIRECTION('',(0.,0.,1.));
#7648=DIRECTION('',(1.,0.,0.));
#7649=DIRECTION('axis',(0.,0.,1.));
#7650=DIRECTION('refdir',(1.,0.,0.));
#7651=DIRECTION('axis',(0.,0.,1.));
#7652=DIRECTION('refdir',(1.,0.,0.));
#7653=DIRECTION('center_axis',(-1.,0.,0.));
#7654=DIRECTION('ref_axis',(0.,0.,1.));
#7655=DIRECTION('',(0.,-1.,0.));
#7656=DIRECTION('',(0.,0.,1.));
#7657=DIRECTION('',(0.,1.,0.));
#7658=DIRECTION('',(0.,0.,-1.));
#7659=DIRECTION('center_axis',(0.,1.,0.));
#7660=DIRECTION('ref_axis',(1.,0.,0.));
#7661=DIRECTION('center_axis',(0.,-1.,0.));
#7662=DIRECTION('ref_axis',(1.,0.,0.));
#7663=DIRECTION('',(-1.,0.,0.));
#7664=DIRECTION('',(0.,0.,1.));
#7665=DIRECTION('center_axis',(1.,0.,0.));
#7666=DIRECTION('ref_axis',(0.,0.,-1.));
#7667=DIRECTION('',(0.,1.,0.));
#7668=DIRECTION('',(0.,1.,0.));
#7669=DIRECTION('',(0.,0.,-1.));
#7670=DIRECTION('center_axis',(0.,0.,1.));
#7671=DIRECTION('ref_axis',(1.,0.,0.));
#7672=DIRECTION('',(1.,0.,0.));
#7673=DIRECTION('center_axis',(0.,1.,0.));
#7674=DIRECTION('ref_axis',(0.,0.,1.));
#7675=DIRECTION('center_axis',(0.,1.,0.));
#7676=DIRECTION('ref_axis',(1.,0.,0.));
#7677=DIRECTION('center_axis',(0.,1.,0.));
#7678=DIRECTION('ref_axis',(1.,0.,0.));
#7679=DIRECTION('center_axis',(0.,1.,0.));
#7680=DIRECTION('ref_axis',(1.,0.,0.));
#7681=DIRECTION('',(0.,-1.,0.));
#7682=DIRECTION('center_axis',(0.,-1.,0.));
#7683=DIRECTION('ref_axis',(1.,0.,0.));
#7684=DIRECTION('center_axis',(0.,1.,0.));
#7685=DIRECTION('ref_axis',(1.,0.,0.));
#7686=DIRECTION('center_axis',(0.,1.,0.));
#7687=DIRECTION('ref_axis',(1.,0.,0.));
#7688=DIRECTION('center_axis',(0.,1.,0.));
#7689=DIRECTION('ref_axis',(1.,0.,0.));
#7690=DIRECTION('center_axis',(0.,1.,0.));
#7691=DIRECTION('ref_axis',(1.,0.,0.));
#7692=DIRECTION('center_axis',(0.,1.,0.));
#7693=DIRECTION('ref_axis',(1.,0.,0.));
#7694=DIRECTION('center_axis',(0.,1.,0.));
#7695=DIRECTION('ref_axis',(1.,0.,0.));
#7696=DIRECTION('center_axis',(0.,-1.,0.));
#7697=DIRECTION('ref_axis',(1.,0.,0.));
#7698=DIRECTION('center_axis',(0.,1.,0.));
#7699=DIRECTION('ref_axis',(1.,0.,0.));
#7700=DIRECTION('',(0.,-1.,0.));
#7701=DIRECTION('center_axis',(0.,1.,0.));
#7702=DIRECTION('ref_axis',(1.,0.,0.));
#7703=DIRECTION('',(0.,-1.,0.));
#7704=DIRECTION('center_axis',(0.,1.,0.));
#7705=DIRECTION('ref_axis',(1.,0.,0.));
#7706=DIRECTION('center_axis',(0.,1.,0.));
#7707=DIRECTION('ref_axis',(1.,0.,0.));
#7708=DIRECTION('center_axis',(0.,1.,0.));
#7709=DIRECTION('ref_axis',(1.,0.,0.));
#7710=DIRECTION('',(0.,-1.,0.));
#7711=DIRECTION('center_axis',(0.,1.,0.));
#7712=DIRECTION('ref_axis',(1.,0.,0.));
#7713=DIRECTION('center_axis',(0.,1.,0.));
#7714=DIRECTION('ref_axis',(1.,0.,0.));
#7715=DIRECTION('axis',(0.,0.,1.));
#7716=DIRECTION('refdir',(1.,0.,0.));
#7717=DIRECTION('center_axis',(0.,1.,0.));
#7718=DIRECTION('ref_axis',(1.,0.,0.));
#7719=DIRECTION('center_axis',(0.,-1.,0.));
#7720=DIRECTION('ref_axis',(1.,0.,0.));
#7721=DIRECTION('',(0.,-1.,0.));
#7722=DIRECTION('center_axis',(0.,-1.,0.));
#7723=DIRECTION('ref_axis',(1.,0.,0.));
#7724=DIRECTION('center_axis',(0.,1.,0.));
#7725=DIRECTION('ref_axis',(1.,0.,0.));
#7726=DIRECTION('center_axis',(0.,1.,0.));
#7727=DIRECTION('ref_axis',(1.,0.,0.));
#7728=DIRECTION('',(0.,-1.,0.));
#7729=DIRECTION('center_axis',(0.,1.,0.));
#7730=DIRECTION('ref_axis',(1.,0.,0.));
#7731=DIRECTION('center_axis',(0.,1.,0.));
#7732=DIRECTION('ref_axis',(1.,0.,0.));
#7733=DIRECTION('center_axis',(0.,1.,0.));
#7734=DIRECTION('ref_axis',(1.,0.,0.));
#7735=DIRECTION('axis',(0.,0.,1.));
#7736=DIRECTION('refdir',(1.,0.,0.));
#7737=DIRECTION('center_axis',(0.,0.,1.));
#7738=DIRECTION('ref_axis',(1.,0.,0.));
#7739=DIRECTION('',(0.,1.,0.));
#7740=DIRECTION('center_axis',(0.,0.,1.));
#7741=DIRECTION('ref_axis',(1.,0.,0.));
#7742=DIRECTION('center_axis',(0.,0.,1.));
#7743=DIRECTION('ref_axis',(1.,0.,0.));
#7744=DIRECTION('center_axis',(0.,0.,1.));
#7745=DIRECTION('ref_axis',(1.,0.,0.));
#7746=DIRECTION('',(0.,0.,1.));
#7747=DIRECTION('center_axis',(0.,0.,1.));
#7748=DIRECTION('ref_axis',(1.,0.,0.));
#7749=DIRECTION('center_axis',(0.,0.,1.));
#7750=DIRECTION('ref_axis',(1.,0.,0.));
#7751=DIRECTION('',(0.,-1.,0.));
#7752=DIRECTION('center_axis',(0.,1.,0.));
#7753=DIRECTION('ref_axis',(1.,0.,0.));
#7754=DIRECTION('center_axis',(0.,-1.,0.));
#7755=DIRECTION('ref_axis',(1.,0.,0.));
#7756=DIRECTION('',(0.,-1.,0.));
#7757=DIRECTION('center_axis',(0.,-1.,0.));
#7758=DIRECTION('ref_axis',(1.,0.,0.));
#7759=DIRECTION('center_axis',(0.,1.,0.));
#7760=DIRECTION('ref_axis',(1.,0.,0.));
#7761=DIRECTION('center_axis',(0.,1.,0.));
#7762=DIRECTION('ref_axis',(1.,0.,0.));
#7763=DIRECTION('',(0.,-1.,0.));
#7764=DIRECTION('center_axis',(0.,1.,0.));
#7765=DIRECTION('ref_axis',(1.,0.,0.));
#7766=DIRECTION('center_axis',(0.,1.,0.));
#7767=DIRECTION('ref_axis',(1.,0.,0.));
#7768=DIRECTION('center_axis',(0.,1.,0.));
#7769=DIRECTION('ref_axis',(1.,0.,0.));
#7770=DIRECTION('axis',(0.,0.,1.));
#7771=DIRECTION('refdir',(1.,0.,0.));
#7772=DIRECTION('center_axis',(0.,0.,1.));
#7773=DIRECTION('ref_axis',(1.,0.,0.));
#7774=DIRECTION('',(0.,1.,0.));
#7775=DIRECTION('center_axis',(0.,0.,1.));
#7776=DIRECTION('ref_axis',(1.,0.,0.));
#7777=DIRECTION('center_axis',(0.,0.,1.));
#7778=DIRECTION('ref_axis',(1.,0.,0.));
#7779=DIRECTION('center_axis',(0.,0.,1.));
#7780=DIRECTION('ref_axis',(1.,0.,0.));
#7781=DIRECTION('',(0.,0.,1.));
#7782=DIRECTION('center_axis',(0.,0.,1.));
#7783=DIRECTION('ref_axis',(1.,0.,0.));
#7784=DIRECTION('center_axis',(0.,0.,1.));
#7785=DIRECTION('ref_axis',(1.,0.,0.));
#7786=DIRECTION('',(0.,-1.,0.));
#7787=DIRECTION('center_axis',(0.,1.,0.));
#7788=DIRECTION('ref_axis',(1.,0.,0.));
#7789=DIRECTION('center_axis',(0.,-1.,0.));
#7790=DIRECTION('ref_axis',(1.,0.,0.));
#7791=DIRECTION('',(0.,-1.,0.));
#7792=DIRECTION('center_axis',(0.,-1.,0.));
#7793=DIRECTION('ref_axis',(1.,0.,0.));
#7794=DIRECTION('center_axis',(0.,1.,0.));
#7795=DIRECTION('ref_axis',(1.,0.,0.));
#7796=DIRECTION('center_axis',(0.,1.,0.));
#7797=DIRECTION('ref_axis',(1.,0.,0.));
#7798=DIRECTION('',(0.,-1.,0.));
#7799=DIRECTION('center_axis',(0.,1.,0.));
#7800=DIRECTION('ref_axis',(1.,0.,0.));
#7801=DIRECTION('center_axis',(0.,1.,0.));
#7802=DIRECTION('ref_axis',(1.,0.,0.));
#7803=DIRECTION('center_axis',(0.,1.,0.));
#7804=DIRECTION('ref_axis',(1.,0.,0.));
#7805=DIRECTION('axis',(0.,0.,1.));
#7806=DIRECTION('refdir',(1.,0.,0.));
#7807=DIRECTION('center_axis',(-1.,0.,0.));
#7808=DIRECTION('ref_axis',(0.,0.,1.));
#7809=DIRECTION('',(0.,0.,1.));
#7810=DIRECTION('',(0.,1.,0.));
#7811=DIRECTION('',(0.,0.,-1.));
#7812=DIRECTION('',(0.,1.,0.));
#7813=DIRECTION('center_axis',(0.,0.,-1.));
#7814=DIRECTION('ref_axis',(-1.,0.,0.));
#7815=DIRECTION('',(-1.,0.,0.));
#7816=DIRECTION('',(0.,1.,0.));
#7817=DIRECTION('',(1.,0.,0.));
#7818=DIRECTION('center_axis',(0.,0.,1.));
#7819=DIRECTION('ref_axis',(1.,0.,0.));
#7820=DIRECTION('center_axis',(1.,0.,0.));
#7821=DIRECTION('ref_axis',(0.,0.,-1.));
#7822=DIRECTION('',(0.,0.,-1.));
#7823=DIRECTION('',(0.,-1.,0.));
#7824=DIRECTION('',(0.,0.,1.));
#7825=DIRECTION('center_axis',(0.,1.,0.));
#7826=DIRECTION('ref_axis',(1.,0.,0.));
#7827=DIRECTION('center_axis',(0.,1.,0.));
#7828=DIRECTION('ref_axis',(1.,0.,0.));
#7829=DIRECTION('center_axis',(0.,-1.,0.));
#7830=DIRECTION('ref_axis',(1.,0.,0.));
#7831=DIRECTION('center_axis',(0.,1.,0.));
#7832=DIRECTION('ref_axis',(-1.83697019872103E-16,0.,1.));
#7833=DIRECTION('center_axis',(0.,1.,0.));
#7834=DIRECTION('ref_axis',(1.,0.,0.));
#7835=DIRECTION('center_axis',(1.,0.,6.12323399573677E-17));
#7836=DIRECTION('ref_axis',(6.12323399573677E-17,0.,-1.));
#7837=DIRECTION('',(1.,0.,6.12323399573677E-17));
#7838=DIRECTION('center_axis',(1.,0.,6.12323399573677E-17));
#7839=DIRECTION('ref_axis',(6.12323399573677E-17,0.,-1.));
#7840=DIRECTION('',(1.,0.,6.12323399573677E-17));
#7841=DIRECTION('center_axis',(0.,-1.,0.));
#7842=DIRECTION('ref_axis',(1.,0.,0.));
#7843=DIRECTION('center_axis',(0.,-1.,0.));
#7844=DIRECTION('ref_axis',(1.,0.,0.));
#7845=DIRECTION('',(0.,1.,0.));
#7846=DIRECTION('',(0.,1.,0.));
#7847=DIRECTION('center_axis',(0.,1.,0.));
#7848=DIRECTION('ref_axis',(1.,0.,0.));
#7849=DIRECTION('center_axis',(0.,0.,1.));
#7850=DIRECTION('ref_axis',(1.,0.,0.));
#7851=DIRECTION('',(0.,0.,1.));
#7852=DIRECTION('center_axis',(0.,0.,1.));
#7853=DIRECTION('ref_axis',(1.,0.,0.));
#7854=DIRECTION('',(0.,0.,1.));
#7855=DIRECTION('center_axis',(0.,1.,0.));
#7856=DIRECTION('ref_axis',(1.,0.,0.));
#7857=DIRECTION('center_axis',(0.,1.,0.));
#7858=DIRECTION('ref_axis',(1.,0.,0.));
#7859=DIRECTION('center_axis',(0.,1.,0.));
#7860=DIRECTION('ref_axis',(1.,0.,0.));
#7861=DIRECTION('center_axis',(0.,1.,0.));
#7862=DIRECTION('ref_axis',(0.987688340595138,0.,0.156434465040231));
#7863=DIRECTION('center_axis',(0.,1.,0.));
#7864=DIRECTION('ref_axis',(1.,0.,0.));
#7865=DIRECTION('center_axis',(0.,1.,0.));
#7866=DIRECTION('ref_axis',(0.951056516295154,0.,0.309016994374948));
#7867=DIRECTION('center_axis',(0.,1.,0.));
#7868=DIRECTION('ref_axis',(1.,0.,0.));
#7869=DIRECTION('center_axis',(0.,1.,0.));
#7870=DIRECTION('ref_axis',(0.891006524188368,0.,0.453990499739547));
#7871=DIRECTION('center_axis',(0.,1.,0.));
#7872=DIRECTION('ref_axis',(1.,0.,0.));
#7873=DIRECTION('center_axis',(0.,1.,0.));
#7874=DIRECTION('ref_axis',(0.809016994374947,0.,0.587785252292473));
#7875=DIRECTION('center_axis',(0.,1.,0.));
#7876=DIRECTION('ref_axis',(1.,0.,0.));
#7877=DIRECTION('center_axis',(0.,1.,0.));
#7878=DIRECTION('ref_axis',(0.707106781186547,0.,0.707106781186548));
#7879=DIRECTION('center_axis',(0.,1.,0.));
#7880=DIRECTION('ref_axis',(1.,0.,0.));
#7881=DIRECTION('center_axis',(0.,1.,0.));
#7882=DIRECTION('ref_axis',(0.587785252292473,0.,0.809016994374948));
#7883=DIRECTION('center_axis',(0.,1.,0.));
#7884=DIRECTION('ref_axis',(1.,0.,0.));
#7885=DIRECTION('center_axis',(0.,1.,0.));
#7886=DIRECTION('ref_axis',(0.453990499739547,0.,0.891006524188368));
#7887=DIRECTION('center_axis',(0.,1.,0.));
#7888=DIRECTION('ref_axis',(1.,0.,0.));
#7889=DIRECTION('center_axis',(0.,1.,0.));
#7890=DIRECTION('ref_axis',(0.309016994374947,0.,0.951056516295154));
#7891=DIRECTION('center_axis',(0.,1.,0.));
#7892=DIRECTION('ref_axis',(1.,0.,0.));
#7893=DIRECTION('center_axis',(0.,1.,0.));
#7894=DIRECTION('ref_axis',(0.156434465040231,0.,0.987688340595138));
#7895=DIRECTION('center_axis',(0.,1.,0.));
#7896=DIRECTION('ref_axis',(1.,0.,0.));
#7897=DIRECTION('center_axis',(0.,1.,0.));
#7898=DIRECTION('ref_axis',(-1.83697019872103E-16,0.,1.));
#7899=DIRECTION('center_axis',(0.,1.,0.));
#7900=DIRECTION('ref_axis',(1.,0.,0.));
#7901=DIRECTION('center_axis',(0.,1.,0.));
#7902=DIRECTION('ref_axis',(-0.156434465040231,0.,0.987688340595138));
#7903=DIRECTION('center_axis',(0.,1.,0.));
#7904=DIRECTION('ref_axis',(1.,0.,0.));
#7905=DIRECTION('center_axis',(0.,1.,0.));
#7906=DIRECTION('ref_axis',(-0.309016994374948,0.,0.951056516295154));
#7907=DIRECTION('center_axis',(0.,1.,0.));
#7908=DIRECTION('ref_axis',(1.,0.,0.));
#7909=DIRECTION('center_axis',(0.,1.,0.));
#7910=DIRECTION('ref_axis',(-0.453990499739547,0.,0.891006524188368));
#7911=DIRECTION('center_axis',(0.,1.,0.));
#7912=DIRECTION('ref_axis',(1.,0.,0.));
#7913=DIRECTION('center_axis',(0.,1.,0.));
#7914=DIRECTION('ref_axis',(-0.587785252292473,0.,0.809016994374947));
#7915=DIRECTION('center_axis',(0.,1.,0.));
#7916=DIRECTION('ref_axis',(1.,0.,0.));
#7917=DIRECTION('center_axis',(0.,1.,0.));
#7918=DIRECTION('ref_axis',(-0.707106781186548,0.,0.707106781186547));
#7919=DIRECTION('center_axis',(0.,1.,0.));
#7920=DIRECTION('ref_axis',(1.,0.,0.));
#7921=DIRECTION('center_axis',(0.,1.,0.));
#7922=DIRECTION('ref_axis',(-0.809016994374947,0.,0.587785252292473));
#7923=DIRECTION('center_axis',(0.,1.,0.));
#7924=DIRECTION('ref_axis',(1.,0.,0.));
#7925=DIRECTION('center_axis',(0.,1.,0.));
#7926=DIRECTION('ref_axis',(-0.891006524188368,0.,0.453990499739547));
#7927=DIRECTION('center_axis',(0.,1.,0.));
#7928=DIRECTION('ref_axis',(1.,0.,0.));
#7929=DIRECTION('center_axis',(0.,1.,0.));
#7930=DIRECTION('ref_axis',(-0.951056516295154,0.,0.309016994374947));
#7931=DIRECTION('center_axis',(0.,1.,0.));
#7932=DIRECTION('ref_axis',(1.,0.,0.));
#7933=DIRECTION('center_axis',(0.,1.,0.));
#7934=DIRECTION('ref_axis',(-0.987688340595138,0.,0.156434465040231));
#7935=DIRECTION('center_axis',(0.,1.,0.));
#7936=DIRECTION('ref_axis',(1.,0.,0.));
#7937=DIRECTION('center_axis',(0.,1.,0.));
#7938=DIRECTION('ref_axis',(-1.,0.,-1.22464679914735E-16));
#7939=DIRECTION('center_axis',(0.,1.,0.));
#7940=DIRECTION('ref_axis',(1.,0.,0.));
#7941=DIRECTION('center_axis',(0.,1.,0.));
#7942=DIRECTION('ref_axis',(-0.987688340595138,0.,-0.156434465040231));
#7943=DIRECTION('center_axis',(0.,1.,0.));
#7944=DIRECTION('ref_axis',(1.,0.,0.));
#7945=DIRECTION('center_axis',(0.,1.,0.));
#7946=DIRECTION('ref_axis',(-0.951056516295154,0.,-0.309016994374948));
#7947=DIRECTION('center_axis',(0.,1.,0.));
#7948=DIRECTION('ref_axis',(1.,0.,0.));
#7949=DIRECTION('center_axis',(0.,1.,0.));
#7950=DIRECTION('ref_axis',(-0.891006524188368,0.,-0.453990499739547));
#7951=DIRECTION('center_axis',(0.,1.,0.));
#7952=DIRECTION('ref_axis',(1.,0.,0.));
#7953=DIRECTION('center_axis',(0.,1.,0.));
#7954=DIRECTION('ref_axis',(-0.809016994374947,0.,-0.587785252292473));
#7955=DIRECTION('center_axis',(0.,1.,0.));
#7956=DIRECTION('ref_axis',(1.,0.,0.));
#7957=DIRECTION('center_axis',(0.,1.,0.));
#7958=DIRECTION('ref_axis',(-0.707106781186547,0.,-0.707106781186548));
#7959=DIRECTION('center_axis',(0.,1.,0.));
#7960=DIRECTION('ref_axis',(1.,0.,0.));
#7961=DIRECTION('center_axis',(0.,1.,0.));
#7962=DIRECTION('ref_axis',(-0.587785252292473,0.,-0.809016994374947));
#7963=DIRECTION('center_axis',(0.,1.,0.));
#7964=DIRECTION('ref_axis',(1.,0.,0.));
#7965=DIRECTION('center_axis',(0.,1.,0.));
#7966=DIRECTION('ref_axis',(-0.453990499739547,0.,-0.891006524188368));
#7967=DIRECTION('center_axis',(0.,1.,0.));
#7968=DIRECTION('ref_axis',(1.,0.,0.));
#7969=DIRECTION('center_axis',(0.,1.,0.));
#7970=DIRECTION('ref_axis',(-0.309016994374947,0.,-0.951056516295154));
#7971=DIRECTION('center_axis',(0.,1.,0.));
#7972=DIRECTION('ref_axis',(1.,0.,0.));
#7973=DIRECTION('center_axis',(0.,1.,0.));
#7974=DIRECTION('ref_axis',(-0.156434465040231,0.,-0.987688340595138));
#7975=DIRECTION('center_axis',(0.,1.,0.));
#7976=DIRECTION('ref_axis',(1.,0.,0.));
#7977=DIRECTION('center_axis',(0.,1.,0.));
#7978=DIRECTION('ref_axis',(6.12323399573677E-17,0.,-1.));
#7979=DIRECTION('center_axis',(0.,1.,0.));
#7980=DIRECTION('ref_axis',(1.,0.,0.));
#7981=DIRECTION('center_axis',(0.,1.,0.));
#7982=DIRECTION('ref_axis',(0.156434465040231,0.,-0.987688340595138));
#7983=DIRECTION('center_axis',(0.,1.,0.));
#7984=DIRECTION('ref_axis',(1.,0.,0.));
#7985=DIRECTION('center_axis',(0.,1.,0.));
#7986=DIRECTION('ref_axis',(0.309016994374948,0.,-0.951056516295154));
#7987=DIRECTION('center_axis',(0.,1.,0.));
#7988=DIRECTION('ref_axis',(1.,0.,0.));
#7989=DIRECTION('center_axis',(0.,1.,0.));
#7990=DIRECTION('ref_axis',(0.453990499739547,0.,-0.891006524188368));
#7991=DIRECTION('center_axis',(0.,1.,0.));
#7992=DIRECTION('ref_axis',(1.,0.,0.));
#7993=DIRECTION('center_axis',(0.,1.,0.));
#7994=DIRECTION('ref_axis',(0.587785252292473,0.,-0.809016994374947));
#7995=DIRECTION('center_axis',(0.,1.,0.));
#7996=DIRECTION('ref_axis',(1.,0.,0.));
#7997=DIRECTION('center_axis',(0.,1.,0.));
#7998=DIRECTION('ref_axis',(0.707106781186548,0.,-0.707106781186547));
#7999=DIRECTION('center_axis',(0.,1.,0.));
#8000=DIRECTION('ref_axis',(1.,0.,0.));
#8001=DIRECTION('center_axis',(0.,1.,0.));
#8002=DIRECTION('ref_axis',(0.809016994374947,0.,-0.587785252292473));
#8003=DIRECTION('center_axis',(0.,1.,0.));
#8004=DIRECTION('ref_axis',(1.,0.,0.));
#8005=DIRECTION('center_axis',(0.,1.,0.));
#8006=DIRECTION('ref_axis',(0.891006524188368,0.,-0.453990499739547));
#8007=DIRECTION('center_axis',(0.,1.,0.));
#8008=DIRECTION('ref_axis',(1.,0.,0.));
#8009=DIRECTION('center_axis',(0.,1.,0.));
#8010=DIRECTION('ref_axis',(0.951056516295154,0.,-0.309016994374947));
#8011=DIRECTION('center_axis',(0.,1.,0.));
#8012=DIRECTION('ref_axis',(1.,0.,0.));
#8013=DIRECTION('center_axis',(0.,1.,0.));
#8014=DIRECTION('ref_axis',(0.987688340595138,0.,-0.156434465040231));
#8015=DIRECTION('center_axis',(0.,1.,0.));
#8016=DIRECTION('ref_axis',(1.,0.,0.));
#8017=DIRECTION('center_axis',(0.,1.,0.));
#8018=DIRECTION('ref_axis',(1.,0.,0.));
#8019=DIRECTION('center_axis',(0.,1.,0.));
#8020=DIRECTION('ref_axis',(1.,0.,0.));
#8021=DIRECTION('center_axis',(0.,-1.,0.));
#8022=DIRECTION('ref_axis',(1.,0.,0.));
#8023=DIRECTION('center_axis',(0.,-1.,0.));
#8024=DIRECTION('ref_axis',(1.,0.,0.));
#8025=DIRECTION('',(0.,1.,0.));
#8026=DIRECTION('center_axis',(0.,1.,0.));
#8027=DIRECTION('ref_axis',(1.,0.,0.));
#8028=DIRECTION('center_axis',(0.,1.,0.));
#8029=DIRECTION('ref_axis',(1.,0.,0.));
#8030=DIRECTION('center_axis',(0.,1.,0.));
#8031=DIRECTION('ref_axis',(1.,0.,0.));
#8032=DIRECTION('center_axis',(0.,-1.,0.));
#8033=DIRECTION('ref_axis',(0.987688340595138,0.,0.156434465040231));
#8034=DIRECTION('center_axis',(0.,1.,0.));
#8035=DIRECTION('ref_axis',(1.,0.,0.));
#8036=DIRECTION('center_axis',(0.,-1.,0.));
#8037=DIRECTION('ref_axis',(1.,0.,0.));
#8038=DIRECTION('center_axis',(0.,1.,0.));
#8039=DIRECTION('ref_axis',(1.,0.,0.));
#8040=DIRECTION('center_axis',(0.,-1.,0.));
#8041=DIRECTION('ref_axis',(0.987688340595138,0.,-0.156434465040231));
#8042=DIRECTION('center_axis',(0.,1.,0.));
#8043=DIRECTION('ref_axis',(1.,0.,0.));
#8044=DIRECTION('center_axis',(0.,-1.,0.));
#8045=DIRECTION('ref_axis',(0.951056516295154,0.,-0.309016994374947));
#8046=DIRECTION('center_axis',(0.,1.,0.));
#8047=DIRECTION('ref_axis',(1.,0.,0.));
#8048=DIRECTION('center_axis',(0.,-1.,0.));
#8049=DIRECTION('ref_axis',(0.891006524188368,0.,-0.453990499739547));
#8050=DIRECTION('center_axis',(0.,1.,0.));
#8051=DIRECTION('ref_axis',(1.,0.,0.));
#8052=DIRECTION('center_axis',(0.,-1.,0.));
#8053=DIRECTION('ref_axis',(0.809016994374947,0.,-0.587785252292473));
#8054=DIRECTION('center_axis',(0.,1.,0.));
#8055=DIRECTION('ref_axis',(1.,0.,0.));
#8056=DIRECTION('center_axis',(0.,-1.,0.));
#8057=DIRECTION('ref_axis',(0.707106781186548,0.,-0.707106781186547));
#8058=DIRECTION('center_axis',(0.,1.,0.));
#8059=DIRECTION('ref_axis',(1.,0.,0.));
#8060=DIRECTION('center_axis',(0.,-1.,0.));
#8061=DIRECTION('ref_axis',(0.587785252292473,0.,-0.809016994374947));
#8062=DIRECTION('center_axis',(0.,1.,0.));
#8063=DIRECTION('ref_axis',(1.,0.,0.));
#8064=DIRECTION('center_axis',(0.,-1.,0.));
#8065=DIRECTION('ref_axis',(0.453990499739547,0.,-0.891006524188368));
#8066=DIRECTION('center_axis',(0.,1.,0.));
#8067=DIRECTION('ref_axis',(1.,0.,0.));
#8068=DIRECTION('center_axis',(0.,-1.,0.));
#8069=DIRECTION('ref_axis',(0.309016994374948,0.,-0.951056516295154));
#8070=DIRECTION('center_axis',(0.,1.,0.));
#8071=DIRECTION('ref_axis',(1.,0.,0.));
#8072=DIRECTION('center_axis',(0.,-1.,0.));
#8073=DIRECTION('ref_axis',(0.156434465040231,0.,-0.987688340595138));
#8074=DIRECTION('center_axis',(0.,1.,0.));
#8075=DIRECTION('ref_axis',(1.,0.,0.));
#8076=DIRECTION('center_axis',(0.,-1.,0.));
#8077=DIRECTION('ref_axis',(6.12323399573677E-17,0.,-1.));
#8078=DIRECTION('center_axis',(0.,1.,0.));
#8079=DIRECTION('ref_axis',(1.,0.,0.));
#8080=DIRECTION('center_axis',(0.,-1.,0.));
#8081=DIRECTION('ref_axis',(-0.156434465040231,0.,-0.987688340595138));
#8082=DIRECTION('center_axis',(0.,1.,0.));
#8083=DIRECTION('ref_axis',(1.,0.,0.));
#8084=DIRECTION('center_axis',(0.,-1.,0.));
#8085=DIRECTION('ref_axis',(-0.309016994374947,0.,-0.951056516295154));
#8086=DIRECTION('center_axis',(0.,1.,0.));
#8087=DIRECTION('ref_axis',(1.,0.,0.));
#8088=DIRECTION('center_axis',(0.,-1.,0.));
#8089=DIRECTION('ref_axis',(-0.453990499739547,0.,-0.891006524188368));
#8090=DIRECTION('center_axis',(0.,1.,0.));
#8091=DIRECTION('ref_axis',(1.,0.,0.));
#8092=DIRECTION('center_axis',(0.,-1.,0.));
#8093=DIRECTION('ref_axis',(-0.587785252292473,0.,-0.809016994374947));
#8094=DIRECTION('center_axis',(0.,1.,0.));
#8095=DIRECTION('ref_axis',(1.,0.,0.));
#8096=DIRECTION('center_axis',(0.,-1.,0.));
#8097=DIRECTION('ref_axis',(-0.707106781186547,0.,-0.707106781186548));
#8098=DIRECTION('center_axis',(0.,1.,0.));
#8099=DIRECTION('ref_axis',(1.,0.,0.));
#8100=DIRECTION('center_axis',(0.,-1.,0.));
#8101=DIRECTION('ref_axis',(-0.809016994374947,0.,-0.587785252292473));
#8102=DIRECTION('center_axis',(0.,1.,0.));
#8103=DIRECTION('ref_axis',(1.,0.,0.));
#8104=DIRECTION('center_axis',(0.,-1.,0.));
#8105=DIRECTION('ref_axis',(-0.891006524188368,0.,-0.453990499739547));
#8106=DIRECTION('center_axis',(0.,1.,0.));
#8107=DIRECTION('ref_axis',(1.,0.,0.));
#8108=DIRECTION('center_axis',(0.,-1.,0.));
#8109=DIRECTION('ref_axis',(-0.951056516295154,0.,-0.309016994374948));
#8110=DIRECTION('center_axis',(0.,1.,0.));
#8111=DIRECTION('ref_axis',(1.,0.,0.));
#8112=DIRECTION('center_axis',(0.,-1.,0.));
#8113=DIRECTION('ref_axis',(-0.987688340595138,0.,-0.156434465040231));
#8114=DIRECTION('center_axis',(0.,1.,0.));
#8115=DIRECTION('ref_axis',(1.,0.,0.));
#8116=DIRECTION('center_axis',(0.,-1.,0.));
#8117=DIRECTION('ref_axis',(-1.,0.,-1.22464679914735E-16));
#8118=DIRECTION('center_axis',(0.,1.,0.));
#8119=DIRECTION('ref_axis',(1.,0.,0.));
#8120=DIRECTION('center_axis',(0.,-1.,0.));
#8121=DIRECTION('ref_axis',(-0.987688340595138,0.,0.156434465040231));
#8122=DIRECTION('center_axis',(0.,1.,0.));
#8123=DIRECTION('ref_axis',(1.,0.,0.));
#8124=DIRECTION('center_axis',(0.,-1.,0.));
#8125=DIRECTION('ref_axis',(-0.951056516295154,0.,0.309016994374947));
#8126=DIRECTION('center_axis',(0.,1.,0.));
#8127=DIRECTION('ref_axis',(1.,0.,0.));
#8128=DIRECTION('center_axis',(0.,-1.,0.));
#8129=DIRECTION('ref_axis',(-0.891006524188368,0.,0.453990499739547));
#8130=DIRECTION('center_axis',(0.,1.,0.));
#8131=DIRECTION('ref_axis',(1.,0.,0.));
#8132=DIRECTION('center_axis',(0.,-1.,0.));
#8133=DIRECTION('ref_axis',(-0.809016994374947,0.,0.587785252292473));
#8134=DIRECTION('center_axis',(0.,1.,0.));
#8135=DIRECTION('ref_axis',(1.,0.,0.));
#8136=DIRECTION('center_axis',(0.,-1.,0.));
#8137=DIRECTION('ref_axis',(-0.707106781186548,0.,0.707106781186547));
#8138=DIRECTION('center_axis',(0.,1.,0.));
#8139=DIRECTION('ref_axis',(1.,0.,0.));
#8140=DIRECTION('center_axis',(0.,-1.,0.));
#8141=DIRECTION('ref_axis',(-0.587785252292473,0.,0.809016994374947));
#8142=DIRECTION('center_axis',(0.,1.,0.));
#8143=DIRECTION('ref_axis',(1.,0.,0.));
#8144=DIRECTION('center_axis',(0.,-1.,0.));
#8145=DIRECTION('ref_axis',(-0.453990499739547,0.,0.891006524188368));
#8146=DIRECTION('center_axis',(0.,1.,0.));
#8147=DIRECTION('ref_axis',(1.,0.,0.));
#8148=DIRECTION('center_axis',(0.,-1.,0.));
#8149=DIRECTION('ref_axis',(-0.309016994374948,0.,0.951056516295154));
#8150=DIRECTION('center_axis',(0.,1.,0.));
#8151=DIRECTION('ref_axis',(1.,0.,0.));
#8152=DIRECTION('center_axis',(0.,-1.,0.));
#8153=DIRECTION('ref_axis',(-0.156434465040231,0.,0.987688340595138));
#8154=DIRECTION('center_axis',(0.,1.,0.));
#8155=DIRECTION('ref_axis',(1.,0.,0.));
#8156=DIRECTION('center_axis',(0.,-1.,0.));
#8157=DIRECTION('ref_axis',(-1.83697019872103E-16,0.,1.));
#8158=DIRECTION('center_axis',(0.,1.,0.));
#8159=DIRECTION('ref_axis',(1.,0.,0.));
#8160=DIRECTION('center_axis',(0.,-1.,0.));
#8161=DIRECTION('ref_axis',(0.156434465040231,0.,0.987688340595138));
#8162=DIRECTION('center_axis',(0.,1.,0.));
#8163=DIRECTION('ref_axis',(1.,0.,0.));
#8164=DIRECTION('center_axis',(0.,-1.,0.));
#8165=DIRECTION('ref_axis',(0.309016994374947,0.,0.951056516295154));
#8166=DIRECTION('center_axis',(0.,1.,0.));
#8167=DIRECTION('ref_axis',(1.,0.,0.));
#8168=DIRECTION('center_axis',(0.,-1.,0.));
#8169=DIRECTION('ref_axis',(0.453990499739547,0.,0.891006524188368));
#8170=DIRECTION('center_axis',(0.,1.,0.));
#8171=DIRECTION('ref_axis',(1.,0.,0.));
#8172=DIRECTION('center_axis',(0.,-1.,0.));
#8173=DIRECTION('ref_axis',(0.587785252292473,0.,0.809016994374948));
#8174=DIRECTION('center_axis',(0.,1.,0.));
#8175=DIRECTION('ref_axis',(1.,0.,0.));
#8176=DIRECTION('center_axis',(0.,-1.,0.));
#8177=DIRECTION('ref_axis',(0.707106781186547,0.,0.707106781186548));
#8178=DIRECTION('center_axis',(0.,1.,0.));
#8179=DIRECTION('ref_axis',(1.,0.,0.));
#8180=DIRECTION('center_axis',(0.,-1.,0.));
#8181=DIRECTION('ref_axis',(0.809016994374947,0.,0.587785252292473));
#8182=DIRECTION('center_axis',(0.,1.,0.));
#8183=DIRECTION('ref_axis',(1.,0.,0.));
#8184=DIRECTION('center_axis',(0.,-1.,0.));
#8185=DIRECTION('ref_axis',(0.891006524188368,0.,0.453990499739547));
#8186=DIRECTION('center_axis',(0.,1.,0.));
#8187=DIRECTION('ref_axis',(1.,0.,0.));
#8188=DIRECTION('center_axis',(0.,-1.,0.));
#8189=DIRECTION('ref_axis',(0.951056516295154,0.,0.309016994374948));
#8190=DIRECTION('center_axis',(0.,1.,0.));
#8191=DIRECTION('ref_axis',(1.,0.,0.));
#8192=DIRECTION('center_axis',(0.,1.,0.));
#8193=DIRECTION('ref_axis',(1.,0.,0.));
#8194=DIRECTION('',(0.,-1.,0.));
#8195=DIRECTION('center_axis',(0.,1.,0.));
#8196=DIRECTION('ref_axis',(-0.987688340595137,0.,-0.156434465040233));
#8197=DIRECTION('',(0.,-1.,0.));
#8198=DIRECTION('',(0.,1.,0.));
#8199=DIRECTION('center_axis',(0.,1.,0.));
#8200=DIRECTION('ref_axis',(1.,0.,0.));
#8201=DIRECTION('',(0.,-1.,0.));
#8202=DIRECTION('center_axis',(0.,1.,0.));
#8203=DIRECTION('ref_axis',(-0.951056516295153,0.,-0.309016994374949));
#8204=DIRECTION('',(0.,1.,0.));
#8205=DIRECTION('center_axis',(0.,1.,0.));
#8206=DIRECTION('ref_axis',(1.,0.,0.));
#8207=DIRECTION('',(0.,-1.,0.));
#8208=DIRECTION('center_axis',(0.,1.,0.));
#8209=DIRECTION('ref_axis',(-0.891006524188368,0.,-0.453990499739547));
#8210=DIRECTION('',(0.,1.,0.));
#8211=DIRECTION('center_axis',(0.,1.,0.));
#8212=DIRECTION('ref_axis',(1.,0.,0.));
#8213=DIRECTION('',(0.,-1.,0.));
#8214=DIRECTION('center_axis',(0.,1.,0.));
#8215=DIRECTION('ref_axis',(-0.809016994374948,0.,-0.587785252292473));
#8216=DIRECTION('',(0.,1.,0.));
#8217=DIRECTION('center_axis',(0.,1.,0.));
#8218=DIRECTION('ref_axis',(1.,0.,0.));
#8219=DIRECTION('',(0.,-1.,0.));
#8220=DIRECTION('center_axis',(0.,1.,0.));
#8221=DIRECTION('ref_axis',(-0.707106781186547,0.,-0.707106781186548));
#8222=DIRECTION('',(0.,1.,0.));
#8223=DIRECTION('center_axis',(0.,1.,0.));
#8224=DIRECTION('ref_axis',(1.,0.,0.));
#8225=DIRECTION('',(0.,-1.,0.));
#8226=DIRECTION('center_axis',(0.,1.,0.));
#8227=DIRECTION('ref_axis',(-0.587785252292474,0.,-0.809016994374947));
#8228=DIRECTION('',(0.,1.,0.));
#8229=DIRECTION('center_axis',(0.,1.,0.));
#8230=DIRECTION('ref_axis',(1.,0.,0.));
#8231=DIRECTION('',(0.,-1.,0.));
#8232=DIRECTION('center_axis',(0.,1.,0.));
#8233=DIRECTION('ref_axis',(-0.453990499739547,0.,-0.891006524188368));
#8234=DIRECTION('',(0.,1.,0.));
#8235=DIRECTION('center_axis',(0.,1.,0.));
#8236=DIRECTION('ref_axis',(1.,0.,0.));
#8237=DIRECTION('',(0.,-1.,0.));
#8238=DIRECTION('center_axis',(0.,1.,0.));
#8239=DIRECTION('ref_axis',(-0.309016994374948,0.,-0.951056516295153));
#8240=DIRECTION('',(0.,1.,0.));
#8241=DIRECTION('center_axis',(0.,1.,0.));
#8242=DIRECTION('ref_axis',(1.,0.,0.));
#8243=DIRECTION('',(0.,-1.,0.));
#8244=DIRECTION('center_axis',(0.,1.,0.));
#8245=DIRECTION('ref_axis',(-0.156434465040232,0.,-0.987688340595138));
#8246=DIRECTION('',(0.,1.,0.));
#8247=DIRECTION('center_axis',(0.,1.,0.));
#8248=DIRECTION('ref_axis',(1.,0.,0.));
#8249=DIRECTION('',(0.,-1.,0.));
#8250=DIRECTION('center_axis',(0.,1.,0.));
#8251=DIRECTION('ref_axis',(3.06161699786838E-16,0.,-1.));
#8252=DIRECTION('',(0.,1.,0.));
#8253=DIRECTION('center_axis',(0.,1.,0.));
#8254=DIRECTION('ref_axis',(1.,0.,0.));
#8255=DIRECTION('',(0.,-1.,0.));
#8256=DIRECTION('center_axis',(0.,1.,0.));
#8257=DIRECTION('ref_axis',(0.156434465040233,0.,-0.987688340595138));
#8258=DIRECTION('',(0.,1.,0.));
#8259=DIRECTION('center_axis',(0.,1.,0.));
#8260=DIRECTION('ref_axis',(1.,0.,0.));
#8261=DIRECTION('',(0.,-1.,0.));
#8262=DIRECTION('center_axis',(0.,1.,0.));
#8263=DIRECTION('ref_axis',(0.309016994374946,0.,-0.951056516295154));
#8264=DIRECTION('',(0.,1.,0.));
#8265=DIRECTION('center_axis',(0.,1.,0.));
#8266=DIRECTION('ref_axis',(1.,0.,0.));
#8267=DIRECTION('',(0.,-1.,0.));
#8268=DIRECTION('center_axis',(0.,1.,0.));
#8269=DIRECTION('ref_axis',(0.453990499739547,0.,-0.891006524188368));
#8270=DIRECTION('',(0.,1.,0.));
#8271=DIRECTION('center_axis',(0.,1.,0.));
#8272=DIRECTION('ref_axis',(1.,0.,0.));
#8273=DIRECTION('',(0.,-1.,0.));
#8274=DIRECTION('center_axis',(0.,1.,0.));
#8275=DIRECTION('ref_axis',(0.587785252292473,0.,-0.809016994374947));
#8276=DIRECTION('',(0.,1.,0.));
#8277=DIRECTION('center_axis',(0.,1.,0.));
#8278=DIRECTION('ref_axis',(1.,0.,0.));
#8279=DIRECTION('',(0.,-1.,0.));
#8280=DIRECTION('center_axis',(0.,1.,0.));
#8281=DIRECTION('ref_axis',(0.707106781186548,0.,-0.707106781186547));
#8282=DIRECTION('',(0.,1.,0.));
#8283=DIRECTION('center_axis',(0.,1.,0.));
#8284=DIRECTION('ref_axis',(1.,0.,0.));
#8285=DIRECTION('',(0.,-1.,0.));
#8286=DIRECTION('center_axis',(0.,1.,0.));
#8287=DIRECTION('ref_axis',(0.809016994374946,0.,-0.587785252292475));
#8288=DIRECTION('',(0.,1.,0.));
#8289=DIRECTION('center_axis',(0.,1.,0.));
#8290=DIRECTION('ref_axis',(1.,0.,0.));
#8291=DIRECTION('',(0.,-1.,0.));
#8292=DIRECTION('center_axis',(0.,1.,0.));
#8293=DIRECTION('ref_axis',(0.891006524188368,0.,-0.453990499739547));
#8294=DIRECTION('',(0.,1.,0.));
#8295=DIRECTION('center_axis',(0.,1.,0.));
#8296=DIRECTION('ref_axis',(1.,0.,0.));
#8297=DIRECTION('',(0.,-1.,0.));
#8298=DIRECTION('center_axis',(0.,1.,0.));
#8299=DIRECTION('ref_axis',(0.951056516295154,0.,-0.309016994374946));
#8300=DIRECTION('',(0.,1.,0.));
#8301=DIRECTION('center_axis',(0.,1.,0.));
#8302=DIRECTION('ref_axis',(1.,0.,0.));
#8303=DIRECTION('',(0.,-1.,0.));
#8304=DIRECTION('center_axis',(0.,1.,0.));
#8305=DIRECTION('ref_axis',(0.987688340595138,0.,-0.156434465040232));
#8306=DIRECTION('',(0.,1.,0.));
#8307=DIRECTION('center_axis',(0.,1.,0.));
#8308=DIRECTION('ref_axis',(1.,0.,0.));
#8309=DIRECTION('',(0.,-1.,0.));
#8310=DIRECTION('center_axis',(0.,1.,0.));
#8311=DIRECTION('ref_axis',(1.,0.,2.44929359829471E-16));
#8312=DIRECTION('',(0.,1.,0.));
#8313=DIRECTION('center_axis',(0.,1.,0.));
#8314=DIRECTION('ref_axis',(1.,0.,0.));
#8315=DIRECTION('',(0.,-1.,0.));
#8316=DIRECTION('center_axis',(0.,1.,0.));
#8317=DIRECTION('ref_axis',(0.987688340595137,0.,0.156434465040232));
#8318=DIRECTION('',(0.,1.,0.));
#8319=DIRECTION('center_axis',(0.,1.,0.));
#8320=DIRECTION('ref_axis',(1.,0.,0.));
#8321=DIRECTION('',(0.,-1.,0.));
#8322=DIRECTION('center_axis',(0.,1.,0.));
#8323=DIRECTION('ref_axis',(0.951056516295154,0.,0.309016994374946));
#8324=DIRECTION('',(0.,1.,0.));
#8325=DIRECTION('center_axis',(0.,1.,0.));
#8326=DIRECTION('ref_axis',(1.,0.,0.));
#8327=DIRECTION('',(0.,-1.,0.));
#8328=DIRECTION('center_axis',(0.,1.,0.));
#8329=DIRECTION('ref_axis',(0.891006524188368,0.,0.453990499739547));
#8330=DIRECTION('',(0.,1.,0.));
#8331=DIRECTION('center_axis',(0.,1.,0.));
#8332=DIRECTION('ref_axis',(1.,0.,0.));
#8333=DIRECTION('',(0.,-1.,0.));
#8334=DIRECTION('center_axis',(0.,1.,0.));
#8335=DIRECTION('ref_axis',(0.809016994374947,0.,0.587785252292473));
#8336=DIRECTION('',(0.,1.,0.));
#8337=DIRECTION('center_axis',(0.,1.,0.));
#8338=DIRECTION('ref_axis',(1.,0.,0.));
#8339=DIRECTION('',(0.,-1.,0.));
#8340=DIRECTION('center_axis',(0.,1.,0.));
#8341=DIRECTION('ref_axis',(0.707106781186547,0.,0.707106781186548));
#8342=DIRECTION('',(0.,1.,0.));
#8343=DIRECTION('center_axis',(0.,1.,0.));
#8344=DIRECTION('ref_axis',(1.,0.,0.));
#8345=DIRECTION('',(0.,-1.,0.));
#8346=DIRECTION('center_axis',(0.,1.,0.));
#8347=DIRECTION('ref_axis',(0.587785252292475,0.,0.809016994374946));
#8348=DIRECTION('',(0.,1.,0.));
#8349=DIRECTION('center_axis',(0.,1.,0.));
#8350=DIRECTION('ref_axis',(1.,0.,0.));
#8351=DIRECTION('',(0.,-1.,0.));
#8352=DIRECTION('center_axis',(0.,1.,0.));
#8353=DIRECTION('ref_axis',(0.453990499739547,0.,0.891006524188368));
#8354=DIRECTION('',(0.,1.,0.));
#8355=DIRECTION('center_axis',(0.,1.,0.));
#8356=DIRECTION('ref_axis',(1.,0.,0.));
#8357=DIRECTION('',(0.,-1.,0.));
#8358=DIRECTION('center_axis',(0.,1.,0.));
#8359=DIRECTION('ref_axis',(0.309016994374946,0.,0.951056516295154));
#8360=DIRECTION('',(0.,1.,0.));
#8361=DIRECTION('center_axis',(0.,1.,0.));
#8362=DIRECTION('ref_axis',(1.,0.,0.));
#8363=DIRECTION('',(0.,-1.,0.));
#8364=DIRECTION('center_axis',(0.,1.,0.));
#8365=DIRECTION('ref_axis',(0.156434465040232,0.,0.987688340595138));
#8366=DIRECTION('',(0.,1.,0.));
#8367=DIRECTION('center_axis',(0.,1.,0.));
#8368=DIRECTION('ref_axis',(1.,0.,0.));
#8369=DIRECTION('',(0.,-1.,0.));
#8370=DIRECTION('center_axis',(0.,1.,0.));
#8371=DIRECTION('ref_axis',(-1.83697019872103E-16,0.,1.));
#8372=DIRECTION('',(0.,1.,0.));
#8373=DIRECTION('center_axis',(0.,1.,0.));
#8374=DIRECTION('ref_axis',(1.,0.,0.));
#8375=DIRECTION('',(0.,-1.,0.));
#8376=DIRECTION('center_axis',(0.,1.,0.));
#8377=DIRECTION('ref_axis',(-0.156434465040232,0.,0.987688340595138));
#8378=DIRECTION('',(0.,1.,0.));
#8379=DIRECTION('center_axis',(0.,1.,0.));
#8380=DIRECTION('ref_axis',(1.,0.,0.));
#8381=DIRECTION('',(0.,-1.,0.));
#8382=DIRECTION('center_axis',(0.,1.,0.));
#8383=DIRECTION('ref_axis',(-0.309016994374946,0.,0.951056516295154));
#8384=DIRECTION('',(0.,1.,0.));
#8385=DIRECTION('center_axis',(0.,1.,0.));
#8386=DIRECTION('ref_axis',(1.,0.,0.));
#8387=DIRECTION('',(0.,-1.,0.));
#8388=DIRECTION('center_axis',(0.,1.,0.));
#8389=DIRECTION('ref_axis',(-0.453990499739549,0.,0.891006524188367));
#8390=DIRECTION('',(0.,1.,0.));
#8391=DIRECTION('center_axis',(0.,1.,0.));
#8392=DIRECTION('ref_axis',(1.,0.,0.));
#8393=DIRECTION('',(0.,-1.,0.));
#8394=DIRECTION('center_axis',(0.,1.,0.));
#8395=DIRECTION('ref_axis',(-0.587785252292474,0.,0.809016994374947));
#8396=DIRECTION('',(0.,1.,0.));
#8397=DIRECTION('center_axis',(0.,1.,0.));
#8398=DIRECTION('ref_axis',(1.,0.,0.));
#8399=DIRECTION('',(0.,-1.,0.));
#8400=DIRECTION('center_axis',(0.,1.,0.));
#8401=DIRECTION('ref_axis',(-0.707106781186548,0.,0.707106781186547));
#8402=DIRECTION('',(0.,1.,0.));
#8403=DIRECTION('center_axis',(0.,1.,0.));
#8404=DIRECTION('ref_axis',(1.,0.,0.));
#8405=DIRECTION('',(0.,-1.,0.));
#8406=DIRECTION('center_axis',(0.,1.,0.));
#8407=DIRECTION('ref_axis',(-0.809016994374947,0.,0.587785252292474));
#8408=DIRECTION('',(0.,1.,0.));
#8409=DIRECTION('center_axis',(0.,1.,0.));
#8410=DIRECTION('ref_axis',(1.,0.,0.));
#8411=DIRECTION('',(0.,-1.,0.));
#8412=DIRECTION('center_axis',(0.,1.,0.));
#8413=DIRECTION('ref_axis',(-0.891006524188368,0.,0.453990499739547));
#8414=DIRECTION('',(0.,1.,0.));
#8415=DIRECTION('center_axis',(0.,1.,0.));
#8416=DIRECTION('ref_axis',(1.,0.,0.));
#8417=DIRECTION('',(0.,-1.,0.));
#8418=DIRECTION('center_axis',(0.,1.,0.));
#8419=DIRECTION('ref_axis',(-0.951056516295154,0.,0.309016994374948));
#8420=DIRECTION('',(0.,1.,0.));
#8421=DIRECTION('center_axis',(0.,1.,0.));
#8422=DIRECTION('ref_axis',(1.,0.,0.));
#8423=DIRECTION('',(0.,-1.,0.));
#8424=DIRECTION('center_axis',(0.,1.,0.));
#8425=DIRECTION('ref_axis',(-0.987688340595137,0.,0.156434465040233));
#8426=DIRECTION('',(0.,1.,0.));
#8427=DIRECTION('center_axis',(0.,1.,0.));
#8428=DIRECTION('ref_axis',(1.,0.,0.));
#8429=DIRECTION('',(0.,1.,0.));
#8430=DIRECTION('center_axis',(0.,1.,0.));
#8431=DIRECTION('ref_axis',(-1.,0.,-1.22464679914735E-16));
#8432=DIRECTION('',(0.,-1.,0.));
#8433=DIRECTION('center_axis',(0.,1.,0.));
#8434=DIRECTION('ref_axis',(1.,0.,0.));
#8435=DIRECTION('axis',(0.,0.,1.));
#8436=DIRECTION('refdir',(1.,0.,0.));
#8437=DIRECTION('center_axis',(1.,0.,0.));
#8438=DIRECTION('ref_axis',(0.,0.,-1.));
#8439=DIRECTION('',(0.,0.707106781186547,-0.707106781186548));
#8440=DIRECTION('',(0.,1.,0.));
#8441=DIRECTION('',(0.,0.707106781186547,0.707106781186548));
#8442=DIRECTION('',(0.,0.,1.));
#8443=DIRECTION('',(0.,-0.707106781186548,0.707106781186548));
#8444=DIRECTION('',(0.,-1.,0.));
#8445=DIRECTION('',(0.,-0.707106781186548,-0.707106781186548));
#8446=DIRECTION('',(0.,0.,-1.));
#8447=DIRECTION('center_axis',(0.,-0.707106781186548,-0.707106781186548));
#8448=DIRECTION('ref_axis',(-1.,0.,0.));
#8449=DIRECTION('',(-1.,0.,0.));
#8450=DIRECTION('',(0.,0.707106781186548,-0.707106781186548));
#8451=DIRECTION('',(1.,0.,0.));
#8452=DIRECTION('center_axis',(0.,-1.,0.));
#8453=DIRECTION('ref_axis',(1.,0.,0.));
#8454=DIRECTION('',(1.,0.,0.));
#8455=DIRECTION('',(0.,0.,-1.));
#8456=DIRECTION('center_axis',(0.,-0.707106781186548,0.707106781186547));
#8457=DIRECTION('ref_axis',(1.,0.,0.));
#8458=DIRECTION('',(-1.,0.,0.));
#8459=DIRECTION('',(0.,-0.707106781186547,-0.707106781186548));
#8460=DIRECTION('center_axis',(0.,0.,1.));
#8461=DIRECTION('ref_axis',(1.,0.,0.));
#8462=DIRECTION('',(1.,0.,0.));
#8463=DIRECTION('',(0.,-1.,0.));
#8464=DIRECTION('center_axis',(1.,0.,0.));
#8465=DIRECTION('ref_axis',(0.,0.,-1.));
#8466=DIRECTION('',(0.,-0.707106781186547,0.707106781186548));
#8467=DIRECTION('',(0.,0.,1.));
#8468=DIRECTION('',(0.,0.707106781186548,0.707106781186548));
#8469=DIRECTION('',(0.,1.,0.));
#8470=DIRECTION('center_axis',(0.,0.707106781186548,0.707106781186547));
#8471=DIRECTION('ref_axis',(1.,0.,0.));
#8472=DIRECTION('',(-1.,0.,0.));
#8473=DIRECTION('center_axis',(0.,1.,0.));
#8474=DIRECTION('ref_axis',(-1.,0.,0.));
#8475=DIRECTION('',(1.,0.,0.));
#8476=DIRECTION('center_axis',(0.,0.707106781186548,-0.707106781186548));
#8477=DIRECTION('ref_axis',(-1.,0.,0.));
#8478=DIRECTION('',(-1.,0.,0.));
#8479=DIRECTION('center_axis',(0.,0.,1.));
#8480=DIRECTION('ref_axis',(1.,0.,0.));
#8481=DIRECTION('axis',(0.,0.,1.));
#8482=DIRECTION('refdir',(1.,0.,0.));
#8483=DIRECTION('center_axis',(0.866025403784439,0.,-0.5));
#8484=DIRECTION('ref_axis',(0.5,0.,0.866025403784439));
#8485=DIRECTION('',(0.5,0.,0.866025403784439));
#8486=DIRECTION('',(0.,-1.,0.));
#8487=DIRECTION('',(0.5,0.,0.866025403784439));
#8488=DIRECTION('',(0.,-1.,0.));
#8489=DIRECTION('center_axis',(1.92296268638356E-16,0.,-1.));
#8490=DIRECTION('ref_axis',(1.,0.,1.92296268638356E-16));
#8491=DIRECTION('',(1.,0.,1.92296268638356E-16));
#8492=DIRECTION('',(0.,-1.,0.));
#8493=DIRECTION('',(1.,0.,1.92296268638356E-16));
#8494=DIRECTION('center_axis',(-0.866025403784439,0.,-0.5));
#8495=DIRECTION('ref_axis',(0.5,0.,-0.866025403784439));
#8496=DIRECTION('',(0.5,0.,-0.866025403784439));
#8497=DIRECTION('',(0.,-1.,0.));
#8498=DIRECTION('',(0.5,0.,-0.866025403784438));
#8499=DIRECTION('center_axis',(-0.866025403784439,0.,0.5));
#8500=DIRECTION('ref_axis',(-0.5,0.,-0.866025403784439));
#8501=DIRECTION('',(-0.5,0.,-0.866025403784439));
#8502=DIRECTION('',(0.,-1.,0.));
#8503=DIRECTION('',(-0.5,0.,-0.866025403784439));
#8504=DIRECTION('center_axis',(-1.92296268638356E-16,0.,1.));
#8505=DIRECTION('ref_axis',(-1.,0.,-1.92296268638356E-16));
#8506=DIRECTION('',(-1.,0.,-1.92296268638356E-16));
#8507=DIRECTION('',(0.,-1.,0.));
#8508=DIRECTION('',(-1.,0.,-1.92296268638356E-16));
#8509=DIRECTION('center_axis',(0.866025403784439,0.,0.5));
#8510=DIRECTION('ref_axis',(-0.5,0.,0.866025403784439));
#8511=DIRECTION('',(-0.5,0.,0.866025403784439));
#8512=DIRECTION('',(-0.5,0.,0.866025403784439));
#8513=DIRECTION('center_axis',(0.,-1.,0.));
#8514=DIRECTION('ref_axis',(0.,0.,-1.));
#8515=DIRECTION('center_axis',(0.,1.,0.));
#8516=DIRECTION('ref_axis',(0.,0.,1.));
#8517=DIRECTION('center_axis',(0.,-1.,0.));
#8518=DIRECTION('ref_axis',(1.,0.,0.));
#8519=DIRECTION('center_axis',(0.,-1.,0.));
#8520=DIRECTION('ref_axis',(1.,0.,0.));
#8521=DIRECTION('center_axis',(0.,-1.,0.));
#8522=DIRECTION('ref_axis',(1.,0.,0.));
#8523=DIRECTION('',(0.707106781186547,0.707106781186548,8.65956056235493E-17));
#8524=DIRECTION('center_axis',(0.,-1.,0.));
#8525=DIRECTION('ref_axis',(1.,0.,0.));
#8526=DIRECTION('center_axis',(0.,1.,0.));
#8527=DIRECTION('ref_axis',(1.,0.,0.));
#8528=DIRECTION('',(0.,1.,0.));
#8529=DIRECTION('center_axis',(0.,1.,0.));
#8530=DIRECTION('ref_axis',(1.,0.,0.));
#8531=DIRECTION('center_axis',(0.,-1.,0.));
#8532=DIRECTION('ref_axis',(1.,0.,0.));
#8533=DIRECTION('',(-0.707106781186547,0.707106781186548,-8.65956056235493E-17));
#8534=DIRECTION('center_axis',(0.,-1.,0.));
#8535=DIRECTION('ref_axis',(0.,0.,-1.));
#8536=DIRECTION('',(0.,0.,1.));
#8537=DIRECTION('',(1.,0.,0.));
#8538=DIRECTION('',(0.,0.,1.));
#8539=DIRECTION('',(1.,0.,0.));
#8540=DIRECTION('',(0.,0.,1.));
#8541=DIRECTION('',(1.,0.,0.));
#8542=DIRECTION('',(0.,0.,1.));
#8543=DIRECTION('',(1.,0.,0.));
#8544=DIRECTION('',(0.,-1.,2.22044604925031E-16));
#8545=DIRECTION('',(1.,0.,0.));
#8546=DIRECTION('',(0.,0.,1.));
#8547=DIRECTION('',(1.,0.,0.));
#8548=DIRECTION('',(8.65956056235493E-17,-8.65956056235493E-17,-1.));
#8549=DIRECTION('',(2.22044604925031E-16,1.,-8.65956056235494E-17));
#8550=DIRECTION('',(0.,-1.,2.22044604925031E-16));
#8551=DIRECTION('',(1.,0.,0.));
#8552=DIRECTION('',(0.,0.,1.));
#8553=DIRECTION('',(1.,0.,0.));
#8554=DIRECTION('',(0.,0.,1.));
#8555=DIRECTION('',(1.,0.,0.));
#8556=CARTESIAN_POINT('',(0.,0.,0.));
#8557=CARTESIAN_POINT('',(0.,0.,0.));
#8558=CARTESIAN_POINT('',(0.,0.,0.));
#8559=CARTESIAN_POINT('Origin',(3.8,1.,-0.1));
#8560=CARTESIAN_POINT('',(3.55,1.,0.));
#8561=CARTESIAN_POINT('Origin',(3.8,1.,0.));
#8562=CARTESIAN_POINT('',(3.55,1.,1.));
#8563=CARTESIAN_POINT('',(3.55,1.,-0.1));
#8564=CARTESIAN_POINT('Origin',(3.8,1.,1.));
#8565=CARTESIAN_POINT('Origin',(-3.8,5.,-0.1));
#8566=CARTESIAN_POINT('',(-4.05,5.,0.));
#8567=CARTESIAN_POINT('Origin',(-3.8,5.,0.));
#8568=CARTESIAN_POINT('',(-4.05,5.,1.));
#8569=CARTESIAN_POINT('',(-4.05,5.,-0.1));
#8570=CARTESIAN_POINT('Origin',(-3.8,5.,1.));
#8571=CARTESIAN_POINT('Origin',(-3.8,1.,-0.1));
#8572=CARTESIAN_POINT('',(-4.05,1.,0.));
#8573=CARTESIAN_POINT('Origin',(-3.8,1.,0.));
#8574=CARTESIAN_POINT('',(-4.05,1.,1.));
#8575=CARTESIAN_POINT('',(-4.05,1.,-0.1));
#8576=CARTESIAN_POINT('Origin',(-3.8,1.,1.));
#8577=CARTESIAN_POINT('Origin',(3.8,5.,-0.1));
#8578=CARTESIAN_POINT('',(3.55,5.,0.));
#8579=CARTESIAN_POINT('Origin',(3.8,5.,0.));
#8580=CARTESIAN_POINT('',(3.55,5.,1.));
#8581=CARTESIAN_POINT('',(3.55,5.,-0.1));
#8582=CARTESIAN_POINT('Origin',(3.8,5.,1.));
#8583=CARTESIAN_POINT('Origin',(5.5,7.,0.));
#8584=CARTESIAN_POINT('',(5.5,7.,0.));
#8585=CARTESIAN_POINT('',(-5.5,7.,0.));
#8586=CARTESIAN_POINT('',(5.5,7.,0.));
#8587=CARTESIAN_POINT('',(-5.5,7.,1.));
#8588=CARTESIAN_POINT('',(-5.5,7.,0.));
#8589=CARTESIAN_POINT('',(5.5,7.,1.));
#8590=CARTESIAN_POINT('',(5.5,7.,1.));
#8591=CARTESIAN_POINT('',(5.5,7.,0.));
#8592=CARTESIAN_POINT('Origin',(5.5,-1.,0.));
#8593=CARTESIAN_POINT('',(5.5,-1.,0.));
#8594=CARTESIAN_POINT('',(5.5,-1.,0.));
#8595=CARTESIAN_POINT('',(5.5,-1.,1.));
#8596=CARTESIAN_POINT('',(5.5,-1.,1.));
#8597=CARTESIAN_POINT('',(5.5,-1.,0.));
#8598=CARTESIAN_POINT('Origin',(-5.5,-1.,0.));
#8599=CARTESIAN_POINT('',(-5.5,-1.,0.));
#8600=CARTESIAN_POINT('',(-5.5,-1.,0.));
#8601=CARTESIAN_POINT('',(-5.5,-1.,1.));
#8602=CARTESIAN_POINT('',(-5.5,-1.,1.));
#8603=CARTESIAN_POINT('',(-5.5,-1.,0.));
#8604=CARTESIAN_POINT('Origin',(-5.5,7.,0.));
#8605=CARTESIAN_POINT('',(-5.5,7.,0.));
#8606=CARTESIAN_POINT('',(-5.5,7.,1.));
#8607=CARTESIAN_POINT('Origin',(0.,3.,1.));
#8608=CARTESIAN_POINT('Origin',(0.,3.,0.));
#8609=CARTESIAN_POINT('',(0.,0.,0.));
#8610=CARTESIAN_POINT('Origin',(-2.8,4.4,4.5));
#8611=CARTESIAN_POINT('',(-2.965,4.4,4.5));
#8612=CARTESIAN_POINT('Origin',(-2.8,4.4,4.5));
#8613=CARTESIAN_POINT('',(-2.965,6.,4.5));
#8614=CARTESIAN_POINT('',(-2.965,4.4,4.5));
#8615=CARTESIAN_POINT('Origin',(-2.8,6.,4.5));
#8616=CARTESIAN_POINT('Origin',(-2.8,4.4,4.5));
#8617=CARTESIAN_POINT('Origin',(1.71450551880629E-16,4.4,7.3));
#8618=CARTESIAN_POINT('',(-0.165,4.4,7.3));
#8619=CARTESIAN_POINT('Origin',(1.71450551880629E-16,4.4,7.3));
#8620=CARTESIAN_POINT('',(-0.165,6.,7.3));
#8621=CARTESIAN_POINT('',(-0.165,4.4,7.3));
#8622=CARTESIAN_POINT('Origin',(1.71450551880629E-16,6.,7.3));
#8623=CARTESIAN_POINT('Origin',(1.66533453693773E-16,4.4,7.3));
#8624=CARTESIAN_POINT('Origin',(2.8,4.4,4.5));
#8625=CARTESIAN_POINT('',(2.635,4.4,4.5));
#8626=CARTESIAN_POINT('Origin',(2.8,4.4,4.5));
#8627=CARTESIAN_POINT('',(2.635,6.,4.5));
#8628=CARTESIAN_POINT('',(2.635,4.4,4.5));
#8629=CARTESIAN_POINT('Origin',(2.8,6.,4.5));
#8630=CARTESIAN_POINT('Origin',(2.8,4.4,4.5));
#8631=CARTESIAN_POINT('Origin',(-5.14351655641888E-16,4.4,1.7));
#8632=CARTESIAN_POINT('',(-0.165000000000001,4.4,1.7));
#8633=CARTESIAN_POINT('Origin',(-5.14351655641888E-16,4.4,1.7));
#8634=CARTESIAN_POINT('',(-0.165000000000001,6.,1.7));
#8635=CARTESIAN_POINT('',(-0.165000000000001,4.4,1.7));
#8636=CARTESIAN_POINT('Origin',(-5.14351655641888E-16,6.,1.7));
#8637=CARTESIAN_POINT('Origin',(-5.27355936696949E-16,4.4,1.7));
#8638=CARTESIAN_POINT('Origin',(-2.8,-0.1,4.5));
#8639=CARTESIAN_POINT('',(-2.965,0.,4.5));
#8640=CARTESIAN_POINT('Origin',(-2.8,0.,4.5));
#8641=CARTESIAN_POINT('',(-2.965,1.6,4.5));
#8642=CARTESIAN_POINT('',(-2.965,-0.1,4.5));
#8643=CARTESIAN_POINT('Origin',(-2.8,1.6,4.5));
#8644=CARTESIAN_POINT('Origin',(-2.8,1.6,4.5));
#8645=CARTESIAN_POINT('Origin',(1.71450551880629E-16,-0.1,7.3));
#8646=CARTESIAN_POINT('',(-0.165,0.,7.3));
#8647=CARTESIAN_POINT('Origin',(1.71450551880629E-16,0.,7.3));
#8648=CARTESIAN_POINT('',(-0.165,1.6,7.3));
#8649=CARTESIAN_POINT('',(-0.165,-0.1,7.3));
#8650=CARTESIAN_POINT('Origin',(1.71450551880629E-16,1.6,7.3));
#8651=CARTESIAN_POINT('Origin',(1.66533453693773E-16,1.6,7.3));
#8652=CARTESIAN_POINT('Origin',(2.8,-0.1,4.5));
#8653=CARTESIAN_POINT('',(2.635,0.,4.5));
#8654=CARTESIAN_POINT('Origin',(2.8,0.,4.5));
#8655=CARTESIAN_POINT('',(2.635,1.6,4.5));
#8656=CARTESIAN_POINT('',(2.635,-0.1,4.5));
#8657=CARTESIAN_POINT('Origin',(2.8,1.6,4.5));
#8658=CARTESIAN_POINT('Origin',(2.8,1.6,4.5));
#8659=CARTESIAN_POINT('Origin',(-5.14351655641888E-16,-0.1,1.7));
#8660=CARTESIAN_POINT('',(-0.165000000000001,0.,1.7));
#8661=CARTESIAN_POINT('Origin',(-5.14351655641888E-16,0.,1.7));
#8662=CARTESIAN_POINT('',(-0.165000000000001,1.6,1.7));
#8663=CARTESIAN_POINT('',(-0.165000000000001,-0.1,1.7));
#8664=CARTESIAN_POINT('Origin',(-5.14351655641888E-16,1.6,1.7));
#8665=CARTESIAN_POINT('Origin',(-5.27355936696949E-16,1.6,1.7));
#8666=CARTESIAN_POINT('Origin',(3.8,1.,0.9));
#8667=CARTESIAN_POINT('',(3.47,1.,1.));
#8668=CARTESIAN_POINT('Origin',(3.8,1.,1.));
#8669=CARTESIAN_POINT('',(3.47,1.,2.5));
#8670=CARTESIAN_POINT('',(3.47,1.,0.9));
#8671=CARTESIAN_POINT('Origin',(3.8,1.,2.5));
#8672=CARTESIAN_POINT('Origin',(-3.8,5.,0.9));
#8673=CARTESIAN_POINT('',(-4.13,5.,1.));
#8674=CARTESIAN_POINT('Origin',(-3.8,5.,1.));
#8675=CARTESIAN_POINT('',(-4.13,5.,2.5));
#8676=CARTESIAN_POINT('',(-4.13,5.,0.9));
#8677=CARTESIAN_POINT('Origin',(-3.8,5.,2.5));
#8678=CARTESIAN_POINT('Origin',(-3.8,1.,0.9));
#8679=CARTESIAN_POINT('',(-4.13,1.,1.));
#8680=CARTESIAN_POINT('Origin',(-3.8,1.,1.));
#8681=CARTESIAN_POINT('',(-4.13,1.,2.5));
#8682=CARTESIAN_POINT('',(-4.13,1.,0.9));
#8683=CARTESIAN_POINT('Origin',(-3.8,1.,2.5));
#8684=CARTESIAN_POINT('Origin',(3.8,5.,0.9));
#8685=CARTESIAN_POINT('',(3.47,5.,1.));
#8686=CARTESIAN_POINT('Origin',(3.8,5.,1.));
#8687=CARTESIAN_POINT('',(3.47,5.,2.5));
#8688=CARTESIAN_POINT('',(3.47,5.,0.9));
#8689=CARTESIAN_POINT('Origin',(3.8,5.,2.5));
#8690=CARTESIAN_POINT('Origin',(0.,5.5,1.75));
#8691=CARTESIAN_POINT('',(2.87228132326901,5.5,2.5));
#8692=CARTESIAN_POINT('',(0.,5.5,1.));
#8693=CARTESIAN_POINT('Origin',(0.,5.5,4.5));
#8694=CARTESIAN_POINT('',(4.5,5.5,2.5));
#8695=CARTESIAN_POINT('',(4.5,5.5,2.5));
#8696=CARTESIAN_POINT('',(4.5,5.5,1.));
#8697=CARTESIAN_POINT('',(4.5,5.5,1.));
#8698=CARTESIAN_POINT('',(-4.5,5.5,1.));
#8699=CARTESIAN_POINT('Origin',(0.,5.5,1.75));
#8700=CARTESIAN_POINT('',(-2.87228132326901,5.5,2.5));
#8701=CARTESIAN_POINT('Origin',(0.,5.5,4.5));
#8702=CARTESIAN_POINT('',(-4.5,5.5,1.));
#8703=CARTESIAN_POINT('',(-4.5,5.5,1.));
#8704=CARTESIAN_POINT('',(-4.5,5.5,2.5));
#8705=CARTESIAN_POINT('',(-4.5,5.5,2.5));
#8706=CARTESIAN_POINT('',(4.5,5.5,2.5));
#8707=CARTESIAN_POINT('Origin',(0.,4.5,1.75));
#8708=CARTESIAN_POINT('',(0.,4.5,1.));
#8709=CARTESIAN_POINT('',(2.87228132326901,4.5,2.5));
#8710=CARTESIAN_POINT('Origin',(0.,4.5,4.5));
#8711=CARTESIAN_POINT('',(4.5,4.5,1.));
#8712=CARTESIAN_POINT('',(-4.5,4.5,1.));
#8713=CARTESIAN_POINT('',(4.5,4.5,2.5));
#8714=CARTESIAN_POINT('',(4.5,4.5,1.));
#8715=CARTESIAN_POINT('',(4.5,4.5,2.5));
#8716=CARTESIAN_POINT('Origin',(0.,4.5,1.75));
#8717=CARTESIAN_POINT('',(-2.87228132326901,4.5,2.5));
#8718=CARTESIAN_POINT('Origin',(0.,4.5,4.5));
#8719=CARTESIAN_POINT('',(-4.5,4.5,2.5));
#8720=CARTESIAN_POINT('',(4.5,4.5,2.5));
#8721=CARTESIAN_POINT('',(-4.5,4.5,1.));
#8722=CARTESIAN_POINT('',(-4.5,4.5,2.5));
#8723=CARTESIAN_POINT('',(-4.5,4.5,1.));
#8724=CARTESIAN_POINT('Origin',(-4.5,4.5,2.5));
#8725=CARTESIAN_POINT('',(2.87228132326901,0.,2.5));
#8726=CARTESIAN_POINT('',(4.5,4.5,2.5));
#8727=CARTESIAN_POINT('Origin',(-4.5,4.5,2.5));
#8728=CARTESIAN_POINT('',(-2.87228132326901,0.,2.5));
#8729=CARTESIAN_POINT('',(-4.5,4.5,2.5));
#8730=CARTESIAN_POINT('Origin',(-4.5,4.5,1.));
#8731=CARTESIAN_POINT('',(-4.5,4.5,1.));
#8732=CARTESIAN_POINT('Origin',(4.5,4.5,1.));
#8733=CARTESIAN_POINT('',(4.5,4.5,1.));
#8734=CARTESIAN_POINT('Origin',(4.5,4.5,2.5));
#8735=CARTESIAN_POINT('Origin',(0.,1.5,1.75));
#8736=CARTESIAN_POINT('',(2.87228132326901,1.5,2.5));
#8737=CARTESIAN_POINT('',(0.,1.5,1.));
#8738=CARTESIAN_POINT('Origin',(0.,1.5,4.5));
#8739=CARTESIAN_POINT('',(4.5,1.5,2.5));
#8740=CARTESIAN_POINT('',(4.5,1.5,2.5));
#8741=CARTESIAN_POINT('',(4.5,1.5,1.));
#8742=CARTESIAN_POINT('',(4.5,1.5,1.));
#8743=CARTESIAN_POINT('',(-4.5,1.5,1.));
#8744=CARTESIAN_POINT('Origin',(0.,1.5,1.75));
#8745=CARTESIAN_POINT('',(-2.87228132326901,1.5,2.5));
#8746=CARTESIAN_POINT('Origin',(0.,1.5,4.5));
#8747=CARTESIAN_POINT('',(-4.5,1.5,1.));
#8748=CARTESIAN_POINT('',(-4.5,1.5,1.));
#8749=CARTESIAN_POINT('',(-4.5,1.5,2.5));
#8750=CARTESIAN_POINT('',(-4.5,1.5,2.5));
#8751=CARTESIAN_POINT('',(4.5,1.5,2.5));
#8752=CARTESIAN_POINT('Origin',(0.,0.5,1.75));
#8753=CARTESIAN_POINT('',(0.,0.5,1.));
#8754=CARTESIAN_POINT('',(2.87228132326901,0.5,2.5));
#8755=CARTESIAN_POINT('Origin',(0.,0.5,4.5));
#8756=CARTESIAN_POINT('',(4.5,0.5,1.));
#8757=CARTESIAN_POINT('',(-4.5,0.5,1.));
#8758=CARTESIAN_POINT('',(4.5,0.5,2.5));
#8759=CARTESIAN_POINT('',(4.5,0.5,1.));
#8760=CARTESIAN_POINT('',(4.5,0.5,2.5));
#8761=CARTESIAN_POINT('Origin',(0.,0.5,1.75));
#8762=CARTESIAN_POINT('',(-2.87228132326901,0.5,2.5));
#8763=CARTESIAN_POINT('Origin',(0.,0.5,4.5));
#8764=CARTESIAN_POINT('',(-4.5,0.5,2.5));
#8765=CARTESIAN_POINT('',(4.5,0.5,2.5));
#8766=CARTESIAN_POINT('',(-4.5,0.5,1.));
#8767=CARTESIAN_POINT('',(-4.5,0.5,2.5));
#8768=CARTESIAN_POINT('',(-4.5,0.5,1.));
#8769=CARTESIAN_POINT('Origin',(-4.5,0.5,2.5));
#8770=CARTESIAN_POINT('',(2.87228132326901,0.,2.5));
#8771=CARTESIAN_POINT('',(4.5,0.5,2.5));
#8772=CARTESIAN_POINT('Origin',(-4.5,0.5,2.5));
#8773=CARTESIAN_POINT('',(-2.87228132326901,0.,2.5));
#8774=CARTESIAN_POINT('',(-4.5,0.5,2.5));
#8775=CARTESIAN_POINT('Origin',(-4.5,0.5,1.));
#8776=CARTESIAN_POINT('',(-4.5,0.5,1.));
#8777=CARTESIAN_POINT('Origin',(4.5,0.5,1.));
#8778=CARTESIAN_POINT('',(4.5,0.5,1.));
#8779=CARTESIAN_POINT('Origin',(4.5,0.5,2.5));
#8780=CARTESIAN_POINT('Origin',(0.,0.,4.5));
#8781=CARTESIAN_POINT('',(-2.35,6.,4.5));
#8782=CARTESIAN_POINT('Origin',(0.,6.,4.5));
#8783=CARTESIAN_POINT('',(-2.35,0.,4.5));
#8784=CARTESIAN_POINT('',(-2.35,0.,4.5));
#8785=CARTESIAN_POINT('Origin',(0.,0.,4.5));
#8786=CARTESIAN_POINT('Origin',(0.,0.,4.5));
#8787=CARTESIAN_POINT('',(-3.5,6.,4.5));
#8788=CARTESIAN_POINT('Origin',(0.,6.,4.5));
#8789=CARTESIAN_POINT('',(-3.5,0.,4.5));
#8790=CARTESIAN_POINT('',(-3.5,0.,4.5));
#8791=CARTESIAN_POINT('Origin',(0.,0.,4.5));
#8792=CARTESIAN_POINT('Origin',(0.,6.,4.5));
#8793=CARTESIAN_POINT('Origin',(0.,0.,4.5));
#8794=CARTESIAN_POINT('',(0.,0.,0.));
#8795=CARTESIAN_POINT('Origin',(0.,1.7,4.5));
#8796=CARTESIAN_POINT('',(-1.75,4.3,4.5));
#8797=CARTESIAN_POINT('Origin',(0.,4.3,4.5));
#8798=CARTESIAN_POINT('',(-1.75,1.7,4.5));
#8799=CARTESIAN_POINT('',(-1.75,1.7,4.5));
#8800=CARTESIAN_POINT('Origin',(0.,1.7,4.5));
#8801=CARTESIAN_POINT('Origin',(0.,1.7,4.5));
#8802=CARTESIAN_POINT('',(-2.34,4.3,4.5));
#8803=CARTESIAN_POINT('Origin',(0.,4.3,4.5));
#8804=CARTESIAN_POINT('',(-2.34,1.7,4.5));
#8805=CARTESIAN_POINT('',(-2.34,1.7,4.5));
#8806=CARTESIAN_POINT('Origin',(0.,1.7,4.5));
#8807=CARTESIAN_POINT('Origin',(0.,4.3,4.5));
#8808=CARTESIAN_POINT('Origin',(0.,1.7,4.5));
#8809=CARTESIAN_POINT('',(0.,0.,0.));
#8810=CARTESIAN_POINT('Origin',(-2.8,-0.5,4.5));
#8811=CARTESIAN_POINT('',(-3.025,-0.4,4.5));
#8812=CARTESIAN_POINT('Origin',(-2.8,-0.4,4.5));
#8813=CARTESIAN_POINT('',(-3.025,0.,4.5));
#8814=CARTESIAN_POINT('',(-3.025,-0.5,4.5));
#8815=CARTESIAN_POINT('Origin',(-2.8,0.,4.5));
#8816=CARTESIAN_POINT('Origin',(1.71450551880629E-16,-0.5,7.3));
#8817=CARTESIAN_POINT('',(-0.225,-0.4,7.3));
#8818=CARTESIAN_POINT('Origin',(1.71450551880629E-16,-0.4,7.3));
#8819=CARTESIAN_POINT('',(-0.225,0.,7.3));
#8820=CARTESIAN_POINT('',(-0.225,-0.5,7.3));
#8821=CARTESIAN_POINT('Origin',(1.71450551880629E-16,0.,7.3));
#8822=CARTESIAN_POINT('Origin',(2.8,-0.5,4.5));
#8823=CARTESIAN_POINT('',(2.575,-0.4,4.5));
#8824=CARTESIAN_POINT('Origin',(2.8,-0.4,4.5));
#8825=CARTESIAN_POINT('',(2.575,0.,4.5));
#8826=CARTESIAN_POINT('',(2.575,-0.5,4.5));
#8827=CARTESIAN_POINT('Origin',(2.8,0.,4.5));
#8828=CARTESIAN_POINT('Origin',(-5.14351655641888E-16,-0.5,1.7));
#8829=CARTESIAN_POINT('',(-0.225000000000001,-0.4,1.7));
#8830=CARTESIAN_POINT('Origin',(-5.14351655641888E-16,-0.4,1.7));
#8831=CARTESIAN_POINT('',(-0.225000000000001,0.,1.7));
#8832=CARTESIAN_POINT('',(-0.225000000000001,-0.5,1.7));
#8833=CARTESIAN_POINT('Origin',(-5.14351655641888E-16,0.,1.7));
#8834=CARTESIAN_POINT('Origin',(0.,0.,4.5));
#8835=CARTESIAN_POINT('',(-2.34,0.3,4.5));
#8836=CARTESIAN_POINT('Origin',(0.,0.3,4.5));
#8837=CARTESIAN_POINT('',(-2.34,0.,4.5));
#8838=CARTESIAN_POINT('',(-2.34,0.,4.5));
#8839=CARTESIAN_POINT('Origin',(0.,0.,4.5));
#8840=CARTESIAN_POINT('Origin',(0.,0.3,4.5));
#8841=CARTESIAN_POINT('',(-1.6,0.3,4.5));
#8842=CARTESIAN_POINT('Origin',(0.,0.3,4.5));
#8843=CARTESIAN_POINT('Origin',(0.,-0.41,4.5));
#8844=CARTESIAN_POINT('',(-1.8,-0.4,4.5));
#8845=CARTESIAN_POINT('Origin',(0.,-0.4,4.5));
#8846=CARTESIAN_POINT('',(-1.8,-0.2,4.5));
#8847=CARTESIAN_POINT('',(-1.8,-0.41,4.5));
#8848=CARTESIAN_POINT('Origin',(0.,-0.2,4.5));
#8849=CARTESIAN_POINT('Origin',(0.,-0.2,4.5));
#8850=CARTESIAN_POINT('',(-1.6,-0.2,4.5));
#8851=CARTESIAN_POINT('Origin',(0.,-0.2,4.5));
#8852=CARTESIAN_POINT('Origin',(0.,-0.4,4.5));
#8853=CARTESIAN_POINT('',(-1.6,-0.4,4.5));
#8854=CARTESIAN_POINT('Origin',(0.,-0.4,4.5));
#8855=CARTESIAN_POINT('',(-3.5,0.,4.5));
#8856=CARTESIAN_POINT('Origin',(0.,0.,4.5));
#8857=CARTESIAN_POINT('',(-3.5,-0.4,4.5));
#8858=CARTESIAN_POINT('',(-3.5,-0.4,4.5));
#8859=CARTESIAN_POINT('Origin',(0.,-0.4,4.5));
#8860=CARTESIAN_POINT('Origin',(0.,0.,4.5));
#8861=CARTESIAN_POINT('Origin',(0.,-0.4,4.5));
#8862=CARTESIAN_POINT('',(0.,0.,0.));
#8863=CARTESIAN_POINT('Origin',(0.,-0.4,4.5));
#8864=CARTESIAN_POINT('',(-1.,-0.2,4.5));
#8865=CARTESIAN_POINT('Origin',(0.,-0.2,4.5));
#8866=CARTESIAN_POINT('',(-1.,-0.4,4.5));
#8867=CARTESIAN_POINT('',(-1.,-0.4,4.5));
#8868=CARTESIAN_POINT('Origin',(0.,-0.4,4.5));
#8869=CARTESIAN_POINT('Origin',(0.,-0.4,4.5));
#8870=CARTESIAN_POINT('',(-1.8,-0.2,4.5));
#8871=CARTESIAN_POINT('Origin',(0.,-0.2,4.5));
#8872=CARTESIAN_POINT('',(-1.8,-0.4,4.5));
#8873=CARTESIAN_POINT('',(-1.8,-0.4,4.5));
#8874=CARTESIAN_POINT('Origin',(0.,-0.4,4.5));
#8875=CARTESIAN_POINT('Origin',(0.,-0.2,4.5));
#8876=CARTESIAN_POINT('Origin',(0.,-0.4,4.5));
#8877=CARTESIAN_POINT('',(0.,0.,0.));
#8878=CARTESIAN_POINT('Origin',(-2.8,5.9,4.5));
#8879=CARTESIAN_POINT('',(-3.025,6.,4.5));
#8880=CARTESIAN_POINT('Origin',(-2.8,6.,4.5));
#8881=CARTESIAN_POINT('',(-3.025,6.4,4.5));
#8882=CARTESIAN_POINT('',(-3.025,5.9,4.5));
#8883=CARTESIAN_POINT('Origin',(-2.8,6.4,4.5));
#8884=CARTESIAN_POINT('Origin',(1.71450551880629E-16,5.9,7.3));
#8885=CARTESIAN_POINT('',(-0.225,6.,7.3));
#8886=CARTESIAN_POINT('Origin',(1.71450551880629E-16,6.,7.3));
#8887=CARTESIAN_POINT('',(-0.225,6.4,7.3));
#8888=CARTESIAN_POINT('',(-0.225,5.9,7.3));
#8889=CARTESIAN_POINT('Origin',(1.71450551880629E-16,6.4,7.3));
#8890=CARTESIAN_POINT('Origin',(2.8,5.9,4.5));
#8891=CARTESIAN_POINT('',(2.575,6.,4.5));
#8892=CARTESIAN_POINT('Origin',(2.8,6.,4.5));
#8893=CARTESIAN_POINT('',(2.575,6.4,4.5));
#8894=CARTESIAN_POINT('',(2.575,5.9,4.5));
#8895=CARTESIAN_POINT('Origin',(2.8,6.4,4.5));
#8896=CARTESIAN_POINT('Origin',(-5.14351655641888E-16,5.9,1.7));
#8897=CARTESIAN_POINT('',(-0.225000000000001,6.,1.7));
#8898=CARTESIAN_POINT('Origin',(-5.14351655641888E-16,6.,1.7));
#8899=CARTESIAN_POINT('',(-0.225000000000001,6.4,1.7));
#8900=CARTESIAN_POINT('',(-0.225000000000001,5.9,1.7));
#8901=CARTESIAN_POINT('Origin',(-5.14351655641888E-16,6.4,1.7));
#8902=CARTESIAN_POINT('Origin',(0.,5.7,4.5));
#8903=CARTESIAN_POINT('',(-2.34,6.,4.5));
#8904=CARTESIAN_POINT('Origin',(0.,6.,4.5));
#8905=CARTESIAN_POINT('',(-2.34,5.7,4.5));
#8906=CARTESIAN_POINT('',(-2.34,5.7,4.5));
#8907=CARTESIAN_POINT('Origin',(0.,5.7,4.5));
#8908=CARTESIAN_POINT('Origin',(0.,5.7,4.5));
#8909=CARTESIAN_POINT('',(-1.8,5.7,4.5));
#8910=CARTESIAN_POINT('Origin',(0.,5.7,4.5));
#8911=CARTESIAN_POINT('Origin',(0.,6.,4.5));
#8912=CARTESIAN_POINT('',(-1.8,6.4,4.5));
#8913=CARTESIAN_POINT('Origin',(0.,6.4,4.5));
#8914=CARTESIAN_POINT('',(-1.8,6.,4.5));
#8915=CARTESIAN_POINT('Origin',(0.,6.,4.5));
#8916=CARTESIAN_POINT('',(-3.5,6.4,4.5));
#8917=CARTESIAN_POINT('Origin',(0.,6.4,4.5));
#8918=CARTESIAN_POINT('',(-3.5,6.,4.5));
#8919=CARTESIAN_POINT('',(-3.5,6.,4.5));
#8920=CARTESIAN_POINT('Origin',(0.,6.,4.5));
#8921=CARTESIAN_POINT('Origin',(0.,6.4,4.5));
#8922=CARTESIAN_POINT('Origin',(0.,6.,4.5));
#8923=CARTESIAN_POINT('',(0.,0.,0.));
#8924=CARTESIAN_POINT('Origin',(5.5,0.,-0.3));
#8925=CARTESIAN_POINT('',(5.5,0.,-0.3));
#8926=CARTESIAN_POINT('',(-5.5,0.,-0.3));
#8927=CARTESIAN_POINT('',(5.5,0.,-0.3));
#8928=CARTESIAN_POINT('',(-5.5,0.,0.));
#8929=CARTESIAN_POINT('',(-5.5,0.,-0.3));
#8930=CARTESIAN_POINT('',(5.5,0.,0.));
#8931=CARTESIAN_POINT('',(5.5,0.,0.));
#8932=CARTESIAN_POINT('',(5.5,0.,-0.3));
#8933=CARTESIAN_POINT('Origin',(5.5,-1.,-0.3));
#8934=CARTESIAN_POINT('',(5.5,-1.,-0.3));
#8935=CARTESIAN_POINT('',(5.5,-1.,-0.3));
#8936=CARTESIAN_POINT('',(5.5,-1.,0.));
#8937=CARTESIAN_POINT('',(5.5,-1.,0.));
#8938=CARTESIAN_POINT('',(5.5,-1.,-0.3));
#8939=CARTESIAN_POINT('Origin',(-5.5,-1.,-0.3));
#8940=CARTESIAN_POINT('',(-5.5,-1.,-0.3));
#8941=CARTESIAN_POINT('',(-5.5,-1.,-0.3));
#8942=CARTESIAN_POINT('',(-5.5,-1.,0.));
#8943=CARTESIAN_POINT('',(-5.5,-1.,0.));
#8944=CARTESIAN_POINT('',(-5.5,-1.,-0.3));
#8945=CARTESIAN_POINT('Origin',(-5.5,0.,-0.3));
#8946=CARTESIAN_POINT('',(-5.5,0.,-0.3));
#8947=CARTESIAN_POINT('',(-5.5,0.,0.));
#8948=CARTESIAN_POINT('Origin',(0.,-0.5,0.));
#8949=CARTESIAN_POINT('Origin',(0.,-0.5,-0.3));
#8950=CARTESIAN_POINT('',(0.,0.,0.));
#8951=CARTESIAN_POINT('Origin',(5.5,7.,-0.3));
#8952=CARTESIAN_POINT('',(5.5,7.,-0.3));
#8953=CARTESIAN_POINT('',(-5.5,7.,-0.3));
#8954=CARTESIAN_POINT('',(5.5,7.,-0.3));
#8955=CARTESIAN_POINT('',(-5.5,7.,0.));
#8956=CARTESIAN_POINT('',(-5.5,7.,-0.3));
#8957=CARTESIAN_POINT('',(5.5,7.,0.));
#8958=CARTESIAN_POINT('',(5.5,7.,0.));
#8959=CARTESIAN_POINT('',(5.5,7.,-0.3));
#8960=CARTESIAN_POINT('Origin',(5.5,6.,-0.3));
#8961=CARTESIAN_POINT('',(5.5,6.,-0.3));
#8962=CARTESIAN_POINT('',(5.5,6.,-0.3));
#8963=CARTESIAN_POINT('',(5.5,6.,0.));
#8964=CARTESIAN_POINT('',(5.5,6.,0.));
#8965=CARTESIAN_POINT('',(5.5,6.,-0.3));
#8966=CARTESIAN_POINT('Origin',(-5.5,6.,-0.3));
#8967=CARTESIAN_POINT('',(-5.5,6.,-0.3));
#8968=CARTESIAN_POINT('',(-5.5,6.,-0.3));
#8969=CARTESIAN_POINT('',(-5.5,6.,0.));
#8970=CARTESIAN_POINT('',(-5.5,6.,0.));
#8971=CARTESIAN_POINT('',(-5.5,6.,-0.3));
#8972=CARTESIAN_POINT('Origin',(-5.5,7.,-0.3));
#8973=CARTESIAN_POINT('',(-5.5,7.,-0.3));
#8974=CARTESIAN_POINT('',(-5.5,7.,0.));
#8975=CARTESIAN_POINT('Origin',(0.,6.5,0.));
#8976=CARTESIAN_POINT('Origin',(0.,6.5,-0.3));
#8977=CARTESIAN_POINT('',(0.,0.,0.));
#8978=CARTESIAN_POINT('',(0.,0.,0.));
#8979=CARTESIAN_POINT('Origin',(0.,0.,0.));
#8980=CARTESIAN_POINT('',(-1.63531,-0.410863395882378,-2.00267715711366E-16));
#8981=CARTESIAN_POINT('',(-2.00267715711366E-16,-0.410863395882378,1.63531));
#8982=CARTESIAN_POINT('Origin',(0.,-0.410863395882378,0.));
#8983=CARTESIAN_POINT('Origin',(0.,-0.410863395882378,0.));
#8984=CARTESIAN_POINT('',(-2.00267715711366E-16,0.410863395882378,1.63531));
#8985=CARTESIAN_POINT('Origin',(-2.05128338857182E-16,0.,1.675));
#8986=CARTESIAN_POINT('',(-1.63531,0.410863395882378,2.00267715711366E-16));
#8987=CARTESIAN_POINT('Origin',(0.,0.410863395882378,0.));
#8988=CARTESIAN_POINT('Origin',(0.,0.410863395882378,0.));
#8989=CARTESIAN_POINT('Origin',(0.,0.,0.));
#8990=CARTESIAN_POINT('',(-1.63531,0.7,-2.00267715711366E-16));
#8991=CARTESIAN_POINT('',(-1.63531,0.,-2.00267715711366E-16));
#8992=CARTESIAN_POINT('Origin',(0.,0.7,0.));
#8993=CARTESIAN_POINT('Origin',(0.,0.,0.));
#8994=CARTESIAN_POINT('',(-1.,-0.6,-1.22464679914735E-16));
#8995=CARTESIAN_POINT('Origin',(0.,-0.6,0.));
#8996=CARTESIAN_POINT('',(-1.,0.6,-1.22464679914735E-16));
#8997=CARTESIAN_POINT('',(-1.,0.,-1.22464679914735E-16));
#8998=CARTESIAN_POINT('Origin',(0.,0.6,0.));
#8999=CARTESIAN_POINT('Origin',(0.,0.65,0.));
#9000=CARTESIAN_POINT('',(-1.1,0.7,-1.34711147906209E-16));
#9001=CARTESIAN_POINT('',(-1.05,0.65,-1.28587913910472E-16));
#9002=CARTESIAN_POINT('Origin',(0.,0.7,0.));
#9003=CARTESIAN_POINT('Origin',(1.63531,0.7,0.));
#9004=CARTESIAN_POINT('Origin',(0.,0.,0.));
#9005=CARTESIAN_POINT('',(-1.63531,-0.7,-2.00267715711366E-16));
#9006=CARTESIAN_POINT('Origin',(0.,-0.7,0.));
#9007=CARTESIAN_POINT('',(-1.63531,0.,-2.00267715711366E-16));
#9008=CARTESIAN_POINT('Origin',(1.1,-0.7,0.));
#9009=CARTESIAN_POINT('',(-1.1,-0.7,-1.34711147906209E-16));
#9010=CARTESIAN_POINT('Origin',(0.,-0.7,0.));
#9011=CARTESIAN_POINT('Origin',(0.,-0.65,0.));
#9012=CARTESIAN_POINT('',(-1.05,-0.65,-1.28587913910472E-16));
#9013=CARTESIAN_POINT('',(0.,0.,0.));
#9014=CARTESIAN_POINT('Origin',(0.,0.,0.));
#9015=CARTESIAN_POINT('',(-1.71469,0.410863395882378,-2.09988962002998E-16));
#9016=CARTESIAN_POINT('',(-2.09988962002998E-16,0.410863395882378,1.71469));
#9017=CARTESIAN_POINT('Origin',(0.,0.410863395882378,0.));
#9018=CARTESIAN_POINT('Origin',(0.,0.410863395882378,0.));
#9019=CARTESIAN_POINT('',(-2.09988962002998E-16,-0.410863395882378,1.71469));
#9020=CARTESIAN_POINT('Origin',(-2.05128338857182E-16,0.,1.675));
#9021=CARTESIAN_POINT('',(-1.71469,-0.410863395882378,2.09988962002998E-16));
#9022=CARTESIAN_POINT('Origin',(0.,-0.410863395882378,0.));
#9023=CARTESIAN_POINT('Origin',(0.,-0.410863395882378,0.));
#9024=CARTESIAN_POINT('Origin',(0.,0.,0.));
#9025=CARTESIAN_POINT('',(-1.71469,-0.7,-2.09988962002998E-16));
#9026=CARTESIAN_POINT('Origin',(0.,-0.7,0.));
#9027=CARTESIAN_POINT('',(-1.71469,0.,-2.09988962002998E-16));
#9028=CARTESIAN_POINT('Origin',(2.25,0.7,0.));
#9029=CARTESIAN_POINT('',(-2.25,0.7,-2.75545529808154E-16));
#9030=CARTESIAN_POINT('Origin',(0.,0.7,0.));
#9031=CARTESIAN_POINT('',(-1.71469,0.7,-2.09988962002998E-16));
#9032=CARTESIAN_POINT('Origin',(0.,0.7,0.));
#9033=CARTESIAN_POINT('Origin',(0.,0.65,0.));
#9034=CARTESIAN_POINT('',(-2.35,0.6,-2.87791997799628E-16));
#9035=CARTESIAN_POINT('Origin',(0.,0.6,0.));
#9036=CARTESIAN_POINT('',(-2.3,0.65,-2.81668763803891E-16));
#9037=CARTESIAN_POINT('Origin',(0.,0.,0.));
#9038=CARTESIAN_POINT('',(-2.35,-0.6,-2.87791997799628E-16));
#9039=CARTESIAN_POINT('Origin',(0.,-0.6,0.));
#9040=CARTESIAN_POINT('',(-2.35,0.,-2.87791997799628E-16));
#9041=CARTESIAN_POINT('Origin',(0.,-0.65,0.));
#9042=CARTESIAN_POINT('',(-2.25,-0.7,-2.75545529808154E-16));
#9043=CARTESIAN_POINT('Origin',(0.,-0.7,0.));
#9044=CARTESIAN_POINT('',(-2.3,-0.65,-2.81668763803891E-16));
#9045=CARTESIAN_POINT('Origin',(1.71469,-0.7,0.));
#9046=CARTESIAN_POINT('Origin',(0.,0.,0.));
#9047=CARTESIAN_POINT('',(-1.71469,0.,-2.09988962002998E-16));
#9048=CARTESIAN_POINT('',(0.,0.,0.));
#9049=CARTESIAN_POINT('Origin',(1.675,0.,0.));
#9050=CARTESIAN_POINT('',(1.675,-2.97627328869245E-33,0.3969));
#9051=CARTESIAN_POINT('',(1.675,-2.97627328869245E-33,-0.3969));
#9052=CARTESIAN_POINT('Origin',(1.675,0.,0.));
#9053=CARTESIAN_POINT('Origin',(1.18440385848747,0.,-1.18440385848747));
#9054=CARTESIAN_POINT('',(1.46505453994041,3.1867025333467E-33,-0.903753177034526));
#9055=CARTESIAN_POINT('',(0.903753177034527,-9.13924911073161E-33,-1.46505453994041));
#9056=CARTESIAN_POINT('Origin',(1.18440385848747,0.,-1.18440385848747));
#9057=CARTESIAN_POINT('Origin',(1.02564169428591E-16,0.,-1.675));
#9058=CARTESIAN_POINT('',(0.3969,-2.97627328869246E-33,-1.675));
#9059=CARTESIAN_POINT('',(-0.3969,-2.97627328869245E-33,-1.675));
#9060=CARTESIAN_POINT('Origin',(1.02564169428591E-16,0.,-1.675));
#9061=CARTESIAN_POINT('Origin',(-1.18440385848747,0.,-1.18440385848747));
#9062=CARTESIAN_POINT('',(-0.903753177034526,3.1867025333467E-33,-1.46505453994041));
#9063=CARTESIAN_POINT('',(-1.46505453994041,-9.13924911073161E-33,-0.903753177034527));
#9064=CARTESIAN_POINT('Origin',(-1.18440385848747,0.,-1.18440385848747));
#9065=CARTESIAN_POINT('Origin',(-1.675,0.,-2.05128338857182E-16));
#9066=CARTESIAN_POINT('',(-1.675,-2.97627328869246E-33,-0.3969));
#9067=CARTESIAN_POINT('',(-1.675,-2.97627328869245E-33,0.3969));
#9068=CARTESIAN_POINT('Origin',(-1.675,0.,-2.05128338857182E-16));
#9069=CARTESIAN_POINT('Origin',(-1.18440385848747,0.,1.18440385848747));
#9070=CARTESIAN_POINT('',(-1.46505453994041,6.26819044436628E-33,0.903753177034526));
#9071=CARTESIAN_POINT('',(-0.903753177034527,-1.22207370217512E-32,1.46505453994041));
#9072=CARTESIAN_POINT('Origin',(-1.18440385848747,0.,1.18440385848747));
#9073=CARTESIAN_POINT('Origin',(-3.07692508285772E-16,0.,1.675));
#9074=CARTESIAN_POINT('',(-0.3969,-2.97627328869246E-33,1.675));
#9075=CARTESIAN_POINT('',(0.396899999999999,-2.97627328869245E-33,1.675));
#9076=CARTESIAN_POINT('Origin',(-3.07692508285772E-16,0.,1.675));
#9077=CARTESIAN_POINT('Origin',(1.18440385848747,0.,1.18440385848747));
#9078=CARTESIAN_POINT('',(0.903753177034526,9.34967835538585E-33,1.46505453994041));
#9079=CARTESIAN_POINT('',(1.46505453994041,-1.53022249327708E-32,0.903753177034527));
#9080=CARTESIAN_POINT('Origin',(1.18440385848747,0.,1.18440385848747));
#9081=CARTESIAN_POINT('',(0.,0.,0.));
#9082=CARTESIAN_POINT('Origin',(1.18440385848747,0.,1.18440385848747));
#9083=CARTESIAN_POINT('',(0.846804978391753,-0.07938,1.40825612658882));
#9084=CARTESIAN_POINT('',(1.40825612658882,-0.07938,0.846804978391754));
#9085=CARTESIAN_POINT('Ctrl Pts',(0.846804978391752,-0.0793800000000001,
1.40825612658882));
#9086=CARTESIAN_POINT('Ctrl Pts',(0.854205272175554,-0.123401821157026,
1.40380622184538));
#9087=CARTESIAN_POINT('Ctrl Pts',(0.867957148219441,-0.166543350814306,
1.39550172959303));
#9088=CARTESIAN_POINT('Ctrl Pts',(0.902193646979982,-0.237231147975234,
1.3735491215176));
#9089=CARTESIAN_POINT('Ctrl Pts',(0.920778333482564,-0.266264900654909,
1.36127834356734));
#9090=CARTESIAN_POINT('Ctrl Pts',(0.962485392528369,-0.317195968905306,
1.33211611256184));
#9091=CARTESIAN_POINT('Ctrl Pts',(0.985600426557816,-0.33909093068465,1.31521005565926));
#9092=CARTESIAN_POINT('Ctrl Pts',(1.03253285680459,-0.373586846396559,1.27866649102984));
#9093=CARTESIAN_POINT('Ctrl Pts',(1.05871835910697,-0.388086240756494,1.25722555095714));
#9094=CARTESIAN_POINT('Ctrl Pts',(1.11153475808518,-0.407068917407805,1.2107812086231));
#9095=CARTESIAN_POINT('Ctrl Pts',(1.13814686046673,-0.411552957311693,1.18575674747573));
#9096=CARTESIAN_POINT('Ctrl Pts',(1.18575674747573,-0.411552957311693,1.13814686046673));
#9097=CARTESIAN_POINT('Ctrl Pts',(1.2107812086231,-0.407068917407805,1.11153475808518));
#9098=CARTESIAN_POINT('Ctrl Pts',(1.25722555095713,-0.388086240756494,1.05871835910697));
#9099=CARTESIAN_POINT('Ctrl Pts',(1.27866649102984,-0.373586846396559,1.03253285680459));
#9100=CARTESIAN_POINT('Ctrl Pts',(1.31521005565926,-0.33909093068465,0.985600426557816));
#9101=CARTESIAN_POINT('Ctrl Pts',(1.33211611256184,-0.317195968905306,0.962485392528369));
#9102=CARTESIAN_POINT('Ctrl Pts',(1.36127834356734,-0.266264900654909,0.920778333482565));
#9103=CARTESIAN_POINT('Ctrl Pts',(1.3735491215176,-0.237231147975234,0.902193646979983));
#9104=CARTESIAN_POINT('Ctrl Pts',(1.39550172959303,-0.166543350814306,0.867957148219442));
#9105=CARTESIAN_POINT('Ctrl Pts',(1.40380622184538,-0.123401821157026,0.854205272175555));
#9106=CARTESIAN_POINT('Ctrl Pts',(1.40825612658882,-0.0793800000000001,
0.846804978391753));
#9107=CARTESIAN_POINT('',(0.886256117232623,-0.07938,1.45861320581289));
#9108=CARTESIAN_POINT('Origin',(1.18440385848747,-0.07938,1.18440385848747));
#9109=CARTESIAN_POINT('',(1.45861320581289,-0.07938,0.886256117232624));
#9110=CARTESIAN_POINT('Ctrl Pts',(1.45861320581289,-0.0793800000000001,
0.886256117232623));
#9111=CARTESIAN_POINT('Ctrl Pts',(1.45630208793976,-0.101649918886749,0.890059788636852));
#9112=CARTESIAN_POINT('Ctrl Pts',(1.45296717977858,-0.123823518623746,0.895520212222107));
#9113=CARTESIAN_POINT('Ctrl Pts',(1.43904931717599,-0.192480977588836,0.917859913453975));
#9114=CARTESIAN_POINT('Ctrl Pts',(1.4243271592157,-0.236152929235938,0.940896403863072));
#9115=CARTESIAN_POINT('Ctrl Pts',(1.39055359345152,-0.303141259068212,0.990027513266106));
#9116=CARTESIAN_POINT('Ctrl Pts',(1.36743459453896,-0.335108247315849,1.02199477007745));
#9117=CARTESIAN_POINT('Ctrl Pts',(1.32643091652006,-0.373243761060364,1.07446535104584));
#9118=CARTESIAN_POINT('Ctrl Pts',(1.30441816675528,-0.387888272594439,1.10126842659597));
#9119=CARTESIAN_POINT('Ctrl Pts',(1.25681160160691,-0.407041111792943,1.15530234155453));
#9120=CARTESIAN_POINT('Ctrl Pts',(1.23119764287622,-0.411552957311693,1.18251418313119));
#9121=CARTESIAN_POINT('Ctrl Pts',(1.18251418313119,-0.411552957311693,1.23119764287622));
#9122=CARTESIAN_POINT('Ctrl Pts',(1.15530234155453,-0.407041111792943,1.25681160160691));
#9123=CARTESIAN_POINT('Ctrl Pts',(1.10126842659597,-0.387888272594439,1.30441816675528));
#9124=CARTESIAN_POINT('Ctrl Pts',(1.07446535104584,-0.373243761060364,1.32643091652006));
#9125=CARTESIAN_POINT('Ctrl Pts',(1.02199477007745,-0.335108247315848,1.36743459453896));
#9126=CARTESIAN_POINT('Ctrl Pts',(0.990027513266105,-0.303141259068211,
1.39055359345152));
#9127=CARTESIAN_POINT('Ctrl Pts',(0.940896403863071,-0.236152929235937,
1.42432715921571));
#9128=CARTESIAN_POINT('Ctrl Pts',(0.917859913453974,-0.192480977588835,
1.43904931717599));
#9129=CARTESIAN_POINT('Ctrl Pts',(0.895520212222106,-0.123823518623745,
1.45296717977858));
#9130=CARTESIAN_POINT('Ctrl Pts',(0.890059788636851,-0.101649918886749,
1.45630208793976));
#9131=CARTESIAN_POINT('Ctrl Pts',(0.886256117232622,-0.0793800000000001,
1.45861320581289));
#9132=CARTESIAN_POINT('Origin',(1.18440385848747,-0.07938,1.18440385848747));
#9133=CARTESIAN_POINT('Origin',(0.,-0.27783,0.));
#9134=CARTESIAN_POINT('',(0.404717578595295,-0.07938,1.65807299932179));
#9135=CARTESIAN_POINT('Origin',(0.,-0.07938,0.));
#9136=CARTESIAN_POINT('',(-0.404717578595296,-0.07938,1.65807299932179));
#9137=CARTESIAN_POINT('Ctrl Pts',(0.404717578595296,-0.0793800000000001,
1.65807299932179));
#9138=CARTESIAN_POINT('Ctrl Pts',(0.400393769631747,-0.101649918886749,
1.65912839404491));
#9139=CARTESIAN_POINT('Ctrl Pts',(0.394174530911058,-0.123823518623745,
1.66063136041479));
#9140=CARTESIAN_POINT('Ctrl Pts',(0.368536561654407,-0.192480977588835,
1.66658649961961));
#9141=CARTESIAN_POINT('Ctrl Pts',(0.341837165343982,-0.236152929235937,
1.67246562047521));
#9142=CARTESIAN_POINT('Ctrl Pts',(0.283214707341173,-0.303141259068211,
1.68332504372461));
#9143=CARTESIAN_POINT('Ctrl Pts',(0.244262842368623,-0.335108247315849,
1.68958170688653));
#9144=CARTESIAN_POINT('Ctrl Pts',(0.178166559972324,-0.373243761060364,
1.69769003172132));
#9145=CARTESIAN_POINT('Ctrl Pts',(0.143648558862931,-0.387888272594439,
1.70107730356824));
#9146=CARTESIAN_POINT('Ctrl Pts',(0.0717778861362652,-0.407041111792943,
1.70562212620408));
#9147=CARTESIAN_POINT('Ctrl Pts',(0.0344244045173309,-0.411552957311693,
1.706752));
#9148=CARTESIAN_POINT('Ctrl Pts',(-0.0344244045173315,-0.411552957311693,
1.706752));
#9149=CARTESIAN_POINT('Ctrl Pts',(-0.0717778861362658,-0.407041111792943,
1.70562212620408));
#9150=CARTESIAN_POINT('Ctrl Pts',(-0.143648558862932,-0.387888272594439,
1.70107730356824));
#9151=CARTESIAN_POINT('Ctrl Pts',(-0.178166559972325,-0.373243761060364,
1.69769003172132));
#9152=CARTESIAN_POINT('Ctrl Pts',(-0.244262842368624,-0.335108247315849,
1.68958170688653));
#9153=CARTESIAN_POINT('Ctrl Pts',(-0.283214707341173,-0.303141259068212,
1.68332504372461));
#9154=CARTESIAN_POINT('Ctrl Pts',(-0.341837165343982,-0.236152929235937,
1.67246562047521));
#9155=CARTESIAN_POINT('Ctrl Pts',(-0.368536561654408,-0.192480977588835,
1.66658649961961));
#9156=CARTESIAN_POINT('Ctrl Pts',(-0.394174530911059,-0.123823518623745,
1.66063136041479));
#9157=CARTESIAN_POINT('Ctrl Pts',(-0.400393769631748,-0.101649918886749,
1.65912839404491));
#9158=CARTESIAN_POINT('Ctrl Pts',(-0.404717578595297,-0.0793800000000001,
1.65807299932179));
#9159=CARTESIAN_POINT('',(-0.886256117232624,-0.07938,1.45861320581289));
#9160=CARTESIAN_POINT('Origin',(0.,-0.07938,0.));
#9161=CARTESIAN_POINT('',(-1.45861320581289,-0.07938,0.886256117232623));
#9162=CARTESIAN_POINT('Ctrl Pts',(-0.886256117232623,-0.0793800000000001,
1.45861320581289));
#9163=CARTESIAN_POINT('Ctrl Pts',(-0.890059788636852,-0.101649918886749,
1.45630208793976));
#9164=CARTESIAN_POINT('Ctrl Pts',(-0.895520212222106,-0.123823518623745,
1.45296717977858));
#9165=CARTESIAN_POINT('Ctrl Pts',(-0.917859913453974,-0.192480977588835,
1.43904931717599));
#9166=CARTESIAN_POINT('Ctrl Pts',(-0.940896403863071,-0.236152929235937,
1.4243271592157));
#9167=CARTESIAN_POINT('Ctrl Pts',(-0.990027513266105,-0.303141259068211,
1.39055359345152));
#9168=CARTESIAN_POINT('Ctrl Pts',(-1.02199477007745,-0.335108247315848,
1.36743459453896));
#9169=CARTESIAN_POINT('Ctrl Pts',(-1.07446535104584,-0.373243761060364,
1.32643091652006));
#9170=CARTESIAN_POINT('Ctrl Pts',(-1.10126842659597,-0.387888272594439,
1.30441816675528));
#9171=CARTESIAN_POINT('Ctrl Pts',(-1.15530234155453,-0.407041111792943,
1.25681160160691));
#9172=CARTESIAN_POINT('Ctrl Pts',(-1.18251418313119,-0.411552957311693,
1.23119764287622));
#9173=CARTESIAN_POINT('Ctrl Pts',(-1.23119764287622,-0.411552957311693,
1.18251418313119));
#9174=CARTESIAN_POINT('Ctrl Pts',(-1.25681160160691,-0.407041111792943,
1.15530234155453));
#9175=CARTESIAN_POINT('Ctrl Pts',(-1.30441816675528,-0.387888272594439,
1.10126842659597));
#9176=CARTESIAN_POINT('Ctrl Pts',(-1.32643091652006,-0.373243761060365,
1.07446535104584));
#9177=CARTESIAN_POINT('Ctrl Pts',(-1.36743459453896,-0.335108247315849,
1.02199477007745));
#9178=CARTESIAN_POINT('Ctrl Pts',(-1.39055359345152,-0.303141259068212,
0.990027513266106));
#9179=CARTESIAN_POINT('Ctrl Pts',(-1.4243271592157,-0.236152929235938,0.940896403863071));
#9180=CARTESIAN_POINT('Ctrl Pts',(-1.43904931717599,-0.192480977588836,
0.917859913453974));
#9181=CARTESIAN_POINT('Ctrl Pts',(-1.45296717977858,-0.123823518623746,
0.895520212222106));
#9182=CARTESIAN_POINT('Ctrl Pts',(-1.45630208793976,-0.101649918886749,
0.890059788636852));
#9183=CARTESIAN_POINT('Ctrl Pts',(-1.45861320581289,-0.0793800000000001,
0.886256117232623));
#9184=CARTESIAN_POINT('',(-1.65807299932179,-0.07938,0.404717578595295));
#9185=CARTESIAN_POINT('Origin',(0.,-0.07938,0.));
#9186=CARTESIAN_POINT('',(-1.706752,-0.411552957311693,2.08591827245526E-16));
#9187=CARTESIAN_POINT('Ctrl Pts',(-1.65807299932179,-0.0793800000000001,
0.404717578595296));
#9188=CARTESIAN_POINT('Ctrl Pts',(-1.65912839404491,-0.101649918886749,
0.400393769631747));
#9189=CARTESIAN_POINT('Ctrl Pts',(-1.66063136041479,-0.123823518623745,
0.394174530911058));
#9190=CARTESIAN_POINT('Ctrl Pts',(-1.66658649961961,-0.192480977588835,
0.368536561654407));
#9191=CARTESIAN_POINT('Ctrl Pts',(-1.67246562047521,-0.236152929235937,
0.341837165343982));
#9192=CARTESIAN_POINT('Ctrl Pts',(-1.68332504372461,-0.303141259068211,
0.283214707341173));
#9193=CARTESIAN_POINT('Ctrl Pts',(-1.68958170688653,-0.335108247315848,
0.244262842368623));
#9194=CARTESIAN_POINT('Ctrl Pts',(-1.69769003172132,-0.373243761060364,
0.178166559972324));
#9195=CARTESIAN_POINT('Ctrl Pts',(-1.70107730356824,-0.387888272594439,
0.143648558862931));
#9196=CARTESIAN_POINT('Ctrl Pts',(-1.70562212620408,-0.407041111792943,
0.0717778861362656));
#9197=CARTESIAN_POINT('Ctrl Pts',(-1.706752,-0.411552957311693,0.0344244045173313));
#9198=CARTESIAN_POINT('Ctrl Pts',(-1.706752,-0.411552957311693,2.08166817117217E-16));
#9199=CARTESIAN_POINT('',(-1.706752,-0.47628,2.09016837373834E-16));
#9200=CARTESIAN_POINT('',(-1.706752,-0.27783,2.09016837373834E-16));
#9201=CARTESIAN_POINT('Origin',(0.,-0.47628,0.));
#9202=CARTESIAN_POINT('',(-1.65807299932179,-0.07938,-0.404717578595296));
#9203=CARTESIAN_POINT('Ctrl Pts',(-1.706752,-0.411552957311693,2.0122792321331E-16));
#9204=CARTESIAN_POINT('Ctrl Pts',(-1.706752,-0.411552957311693,-0.0344244045173309));
#9205=CARTESIAN_POINT('Ctrl Pts',(-1.70562212620408,-0.407041111792943,
-0.0717778861362652));
#9206=CARTESIAN_POINT('Ctrl Pts',(-1.70107730356824,-0.387888272594439,
-0.143648558862931));
#9207=CARTESIAN_POINT('Ctrl Pts',(-1.69769003172132,-0.373243761060365,
-0.178166559972324));
#9208=CARTESIAN_POINT('Ctrl Pts',(-1.68958170688653,-0.335108247315849,
-0.244262842368623));
#9209=CARTESIAN_POINT('Ctrl Pts',(-1.68332504372461,-0.303141259068212,
-0.283214707341173));
#9210=CARTESIAN_POINT('Ctrl Pts',(-1.67246562047521,-0.236152929235938,
-0.341837165343982));
#9211=CARTESIAN_POINT('Ctrl Pts',(-1.66658649961961,-0.192480977588836,
-0.368536561654407));
#9212=CARTESIAN_POINT('Ctrl Pts',(-1.66063136041479,-0.123823518623745,
-0.394174530911059));
#9213=CARTESIAN_POINT('Ctrl Pts',(-1.65912839404491,-0.101649918886749,
-0.400393769631748));
#9214=CARTESIAN_POINT('Ctrl Pts',(-1.65807299932179,-0.0793800000000001,
-0.404717578595296));
#9215=CARTESIAN_POINT('',(-1.45861320581289,-0.07938,-0.886256117232623));
#9216=CARTESIAN_POINT('Origin',(0.,-0.07938,0.));
#9217=CARTESIAN_POINT('',(-0.886256117232623,-0.07938,-1.45861320581289));
#9218=CARTESIAN_POINT('Ctrl Pts',(-1.45861320581289,-0.0793800000000001,
-0.886256117232623));
#9219=CARTESIAN_POINT('Ctrl Pts',(-1.45630208793976,-0.101649918886749,
-0.890059788636852));
#9220=CARTESIAN_POINT('Ctrl Pts',(-1.45296717977858,-0.123823518623745,
-0.895520212222106));
#9221=CARTESIAN_POINT('Ctrl Pts',(-1.43904931717599,-0.192480977588835,
-0.917859913453974));
#9222=CARTESIAN_POINT('Ctrl Pts',(-1.4243271592157,-0.236152929235937,-0.940896403863072));
#9223=CARTESIAN_POINT('Ctrl Pts',(-1.39055359345152,-0.303141259068212,
-0.990027513266106));
#9224=CARTESIAN_POINT('Ctrl Pts',(-1.36743459453896,-0.335108247315849,
-1.02199477007745));
#9225=CARTESIAN_POINT('Ctrl Pts',(-1.32643091652006,-0.373243761060364,
-1.07446535104584));
#9226=CARTESIAN_POINT('Ctrl Pts',(-1.30441816675528,-0.387888272594439,
-1.10126842659597));
#9227=CARTESIAN_POINT('Ctrl Pts',(-1.25681160160691,-0.407041111792943,
-1.15530234155453));
#9228=CARTESIAN_POINT('Ctrl Pts',(-1.23119764287622,-0.411552957311693,
-1.18251418313119));
#9229=CARTESIAN_POINT('Ctrl Pts',(-1.18251418313119,-0.411552957311693,
-1.23119764287622));
#9230=CARTESIAN_POINT('Ctrl Pts',(-1.15530234155453,-0.407041111792943,
-1.25681160160691));
#9231=CARTESIAN_POINT('Ctrl Pts',(-1.10126842659597,-0.387888272594439,
-1.30441816675528));
#9232=CARTESIAN_POINT('Ctrl Pts',(-1.07446535104584,-0.373243761060364,
-1.32643091652006));
#9233=CARTESIAN_POINT('Ctrl Pts',(-1.02199477007745,-0.335108247315848,
-1.36743459453896));
#9234=CARTESIAN_POINT('Ctrl Pts',(-0.990027513266105,-0.303141259068211,
-1.39055359345152));
#9235=CARTESIAN_POINT('Ctrl Pts',(-0.940896403863071,-0.236152929235936,
-1.42432715921571));
#9236=CARTESIAN_POINT('Ctrl Pts',(-0.917859913453974,-0.192480977588835,
-1.43904931717599));
#9237=CARTESIAN_POINT('Ctrl Pts',(-0.895520212222106,-0.123823518623745,
-1.45296717977858));
#9238=CARTESIAN_POINT('Ctrl Pts',(-0.890059788636851,-0.101649918886749,
-1.45630208793976));
#9239=CARTESIAN_POINT('Ctrl Pts',(-0.886256117232623,-0.0793800000000001,
-1.45861320581289));
#9240=CARTESIAN_POINT('',(-0.404717578595295,-0.07938,-1.65807299932179));
#9241=CARTESIAN_POINT('Origin',(0.,-0.07938,0.));
#9242=CARTESIAN_POINT('',(0.404717578595296,-0.07938,-1.65807299932179));
#9243=CARTESIAN_POINT('Ctrl Pts',(-0.404717578595296,-0.0793800000000001,
-1.65807299932179));
#9244=CARTESIAN_POINT('Ctrl Pts',(-0.400393769631747,-0.101649918886749,
-1.65912839404491));
#9245=CARTESIAN_POINT('Ctrl Pts',(-0.394174530911058,-0.123823518623746,
-1.66063136041479));
#9246=CARTESIAN_POINT('Ctrl Pts',(-0.368536561654407,-0.192480977588836,
-1.66658649961961));
#9247=CARTESIAN_POINT('Ctrl Pts',(-0.341837165343982,-0.236152929235938,
-1.67246562047521));
#9248=CARTESIAN_POINT('Ctrl Pts',(-0.283214707341173,-0.303141259068212,
-1.68332504372461));
#9249=CARTESIAN_POINT('Ctrl Pts',(-0.244262842368623,-0.335108247315849,
-1.68958170688653));
#9250=CARTESIAN_POINT('Ctrl Pts',(-0.178166559972324,-0.373243761060364,
-1.69769003172132));
#9251=CARTESIAN_POINT('Ctrl Pts',(-0.143648558862931,-0.387888272594439,
-1.70107730356824));
#9252=CARTESIAN_POINT('Ctrl Pts',(-0.0717778861362653,-0.407041111792943,
-1.70562212620408));
#9253=CARTESIAN_POINT('Ctrl Pts',(-0.034424404517331,-0.411552957311693,
-1.706752));
#9254=CARTESIAN_POINT('Ctrl Pts',(0.0344244045173312,-0.411552957311693,
-1.706752));
#9255=CARTESIAN_POINT('Ctrl Pts',(0.0717778861362655,-0.407041111792943,
-1.70562212620408));
#9256=CARTESIAN_POINT('Ctrl Pts',(0.143648558862931,-0.387888272594439,
-1.70107730356824));
#9257=CARTESIAN_POINT('Ctrl Pts',(0.178166559972324,-0.373243761060364,
-1.69769003172132));
#9258=CARTESIAN_POINT('Ctrl Pts',(0.244262842368623,-0.335108247315849,
-1.68958170688653));
#9259=CARTESIAN_POINT('Ctrl Pts',(0.283214707341173,-0.303141259068212,
-1.68332504372461));
#9260=CARTESIAN_POINT('Ctrl Pts',(0.341837165343982,-0.236152929235937,
-1.67246562047521));
#9261=CARTESIAN_POINT('Ctrl Pts',(0.368536561654407,-0.192480977588835,
-1.66658649961961));
#9262=CARTESIAN_POINT('Ctrl Pts',(0.394174530911059,-0.123823518623745,
-1.66063136041479));
#9263=CARTESIAN_POINT('Ctrl Pts',(0.400393769631748,-0.101649918886749,
-1.65912839404491));
#9264=CARTESIAN_POINT('Ctrl Pts',(0.404717578595296,-0.0793800000000001,
-1.65807299932179));
#9265=CARTESIAN_POINT('',(0.886256117232623,-0.07938,-1.45861320581289));
#9266=CARTESIAN_POINT('Origin',(0.,-0.07938,0.));
#9267=CARTESIAN_POINT('',(1.45861320581289,-0.07938,-0.886256117232623));
#9268=CARTESIAN_POINT('Ctrl Pts',(0.886256117232623,-0.0793800000000001,
-1.45861320581289));
#9269=CARTESIAN_POINT('Ctrl Pts',(0.890059788636852,-0.101649918886749,
-1.45630208793976));
#9270=CARTESIAN_POINT('Ctrl Pts',(0.895520212222106,-0.123823518623745,
-1.45296717977858));
#9271=CARTESIAN_POINT('Ctrl Pts',(0.917859913453974,-0.192480977588835,
-1.43904931717599));
#9272=CARTESIAN_POINT('Ctrl Pts',(0.940896403863072,-0.236152929235937,
-1.4243271592157));
#9273=CARTESIAN_POINT('Ctrl Pts',(0.990027513266106,-0.303141259068211,
-1.39055359345152));
#9274=CARTESIAN_POINT('Ctrl Pts',(1.02199477007745,-0.335108247315849,-1.36743459453896));
#9275=CARTESIAN_POINT('Ctrl Pts',(1.07446535104584,-0.373243761060364,-1.32643091652006));
#9276=CARTESIAN_POINT('Ctrl Pts',(1.10126842659597,-0.387888272594439,-1.30441816675528));
#9277=CARTESIAN_POINT('Ctrl Pts',(1.15530234155453,-0.407041111792943,-1.25681160160691));
#9278=CARTESIAN_POINT('Ctrl Pts',(1.18251418313119,-0.411552957311693,-1.23119764287622));
#9279=CARTESIAN_POINT('Ctrl Pts',(1.23119764287622,-0.411552957311693,-1.18251418313119));
#9280=CARTESIAN_POINT('Ctrl Pts',(1.25681160160691,-0.407041111792943,-1.15530234155453));
#9281=CARTESIAN_POINT('Ctrl Pts',(1.30441816675528,-0.387888272594439,-1.10126842659597));
#9282=CARTESIAN_POINT('Ctrl Pts',(1.32643091652006,-0.373243761060364,-1.07446535104584));
#9283=CARTESIAN_POINT('Ctrl Pts',(1.36743459453896,-0.335108247315849,-1.02199477007745));
#9284=CARTESIAN_POINT('Ctrl Pts',(1.39055359345152,-0.303141259068212,-0.990027513266105));
#9285=CARTESIAN_POINT('Ctrl Pts',(1.4243271592157,-0.236152929235937,-0.940896403863071));
#9286=CARTESIAN_POINT('Ctrl Pts',(1.43904931717599,-0.192480977588835,-0.917859913453974));
#9287=CARTESIAN_POINT('Ctrl Pts',(1.45296717977858,-0.123823518623745,-0.895520212222106));
#9288=CARTESIAN_POINT('Ctrl Pts',(1.45630208793976,-0.101649918886749,-0.890059788636852));
#9289=CARTESIAN_POINT('Ctrl Pts',(1.45861320581289,-0.0793800000000001,
-0.886256117232623));
#9290=CARTESIAN_POINT('',(1.65807299932179,-0.07938,-0.404717578595296));
#9291=CARTESIAN_POINT('Origin',(0.,-0.07938,0.));
#9292=CARTESIAN_POINT('',(1.65807299932179,-0.07938,0.404717578595296));
#9293=CARTESIAN_POINT('Ctrl Pts',(1.65807299932179,-0.0793800000000001,
-0.404717578595296));
#9294=CARTESIAN_POINT('Ctrl Pts',(1.65912839404491,-0.101649918886749,-0.400393769631747));
#9295=CARTESIAN_POINT('Ctrl Pts',(1.66063136041479,-0.123823518623745,-0.394174530911058));
#9296=CARTESIAN_POINT('Ctrl Pts',(1.66658649961961,-0.192480977588835,-0.368536561654407));
#9297=CARTESIAN_POINT('Ctrl Pts',(1.67246562047521,-0.236152929235937,-0.341837165343982));
#9298=CARTESIAN_POINT('Ctrl Pts',(1.68332504372461,-0.303141259068212,-0.283214707341173));
#9299=CARTESIAN_POINT('Ctrl Pts',(1.68958170688653,-0.335108247315849,-0.244262842368623));
#9300=CARTESIAN_POINT('Ctrl Pts',(1.69769003172132,-0.373243761060364,-0.178166559972324));
#9301=CARTESIAN_POINT('Ctrl Pts',(1.70107730356824,-0.387888272594439,-0.143648558862931));
#9302=CARTESIAN_POINT('Ctrl Pts',(1.70562212620408,-0.407041111792943,-0.0717778861362655));
#9303=CARTESIAN_POINT('Ctrl Pts',(1.706752,-0.411552957311693,-0.0344244045173312));
#9304=CARTESIAN_POINT('Ctrl Pts',(1.706752,-0.411552957311693,0.0344244045173312));
#9305=CARTESIAN_POINT('Ctrl Pts',(1.70562212620408,-0.407041111792943,0.0717778861362655));
#9306=CARTESIAN_POINT('Ctrl Pts',(1.70107730356824,-0.387888272594439,0.143648558862931));
#9307=CARTESIAN_POINT('Ctrl Pts',(1.69769003172132,-0.373243761060364,0.178166559972324));
#9308=CARTESIAN_POINT('Ctrl Pts',(1.68958170688653,-0.335108247315849,0.244262842368623));
#9309=CARTESIAN_POINT('Ctrl Pts',(1.68332504372461,-0.303141259068212,0.283214707341173));
#9310=CARTESIAN_POINT('Ctrl Pts',(1.67246562047521,-0.236152929235937,0.341837165343982));
#9311=CARTESIAN_POINT('Ctrl Pts',(1.66658649961961,-0.192480977588835,0.368536561654407));
#9312=CARTESIAN_POINT('Ctrl Pts',(1.66063136041479,-0.123823518623745,0.394174530911058));
#9313=CARTESIAN_POINT('Ctrl Pts',(1.65912839404491,-0.101649918886749,0.400393769631747));
#9314=CARTESIAN_POINT('Ctrl Pts',(1.65807299932179,-0.0793800000000001,
0.404717578595296));
#9315=CARTESIAN_POINT('Origin',(0.,-0.07938,0.));
#9316=CARTESIAN_POINT('Origin',(0.,-0.07938,0.));
#9317=CARTESIAN_POINT('',(0.397005914195118,-0.07938,1.59456899932179));
#9318=CARTESIAN_POINT('Origin',(0.,-0.07938,0.));
#9319=CARTESIAN_POINT('Origin',(-3.33066907387547E-16,-0.07938,1.675));
#9320=CARTESIAN_POINT('Origin',(-3.33066907387547E-16,0.,1.675));
#9321=CARTESIAN_POINT('',(-0.397005914195118,-0.07938,1.59456899932179));
#9322=CARTESIAN_POINT('Ctrl Pts',(-0.397005914195119,-0.0793800000000001,
1.59456899932179));
#9323=CARTESIAN_POINT('Ctrl Pts',(-0.3886265584581,-0.123401821157026,1.59665523941937));
#9324=CARTESIAN_POINT('Ctrl Pts',(-0.373030350867485,-0.166543350814306,
1.60050712143809));
#9325=CARTESIAN_POINT('Ctrl Pts',(-0.333298652394954,-0.237231147975234,
1.60919314384089));
#9326=CARTESIAN_POINT('Ctrl Pts',(-0.311480544243687,-0.266264900654909,
1.61365775139403));
#9327=CARTESIAN_POINT('Ctrl Pts',(-0.261368388670537,-0.317195968905306,
1.62252828437015));
#9328=CARTESIAN_POINT('Ctrl Pts',(-0.233069203882014,-0.33909093068465,
1.62691869420078));
#9329=CARTESIAN_POINT('Ctrl Pts',(-0.174042761838764,-0.373586846396559,
1.63426473152765));
#9330=CARTESIAN_POINT('Ctrl Pts',(-0.14036578147155,-0.388086240756494,
1.63761964365402));
#9331=CARTESIAN_POINT('Ctrl Pts',(-0.0701778381840615,-0.407068917407805,
1.64212536811722));
#9332=CARTESIAN_POINT('Ctrl Pts',(-0.0336652739555918,-0.411552957311693,
1.643248));
#9333=CARTESIAN_POINT('Ctrl Pts',(0.0336652739555913,-0.411552957311693,
1.643248));
#9334=CARTESIAN_POINT('Ctrl Pts',(0.070177838184061,-0.407068917407805,
1.64212536811722));
#9335=CARTESIAN_POINT('Ctrl Pts',(0.140365781471549,-0.388086240756494,
1.63761964365402));
#9336=CARTESIAN_POINT('Ctrl Pts',(0.174042761838763,-0.373586846396559,
1.63426473152765));
#9337=CARTESIAN_POINT('Ctrl Pts',(0.233069203882014,-0.33909093068465,1.62691869420078));
#9338=CARTESIAN_POINT('Ctrl Pts',(0.261368388670536,-0.317195968905306,
1.62252828437015));
#9339=CARTESIAN_POINT('Ctrl Pts',(0.311480544243686,-0.266264900654908,
1.61365775139403));
#9340=CARTESIAN_POINT('Ctrl Pts',(0.333298652394954,-0.237231147975234,
1.60919314384089));
#9341=CARTESIAN_POINT('Ctrl Pts',(0.373030350867484,-0.166543350814306,
1.60050712143809));
#9342=CARTESIAN_POINT('Ctrl Pts',(0.388626558458099,-0.123401821157026,
1.59665523941937));
#9343=CARTESIAN_POINT('Ctrl Pts',(0.397005914195118,-0.07938,1.59456899932179));
#9344=CARTESIAN_POINT('Origin',(-3.33066907387547E-16,-0.07938,1.675));
#9345=CARTESIAN_POINT('Origin',(0.,-0.07938,0.));
#9346=CARTESIAN_POINT('',(-0.846804978391754,-0.07938,1.40825612658882));
#9347=CARTESIAN_POINT('Origin',(0.,-0.07938,0.));
#9348=CARTESIAN_POINT('Origin',(-1.18440385848747,-0.07938,1.18440385848747));
#9349=CARTESIAN_POINT('Origin',(-1.18440385848747,0.,1.18440385848747));
#9350=CARTESIAN_POINT('',(-1.40825612658882,-0.07938,0.846804978391753));
#9351=CARTESIAN_POINT('Ctrl Pts',(-1.40825612658882,-0.0793800000000001,
0.846804978391753));
#9352=CARTESIAN_POINT('Ctrl Pts',(-1.40380622184538,-0.123401821157026,
0.854205272175555));
#9353=CARTESIAN_POINT('Ctrl Pts',(-1.39550172959303,-0.166543350814306,
0.867957148219442));
#9354=CARTESIAN_POINT('Ctrl Pts',(-1.3735491215176,-0.237231147975235,0.902193646979983));
#9355=CARTESIAN_POINT('Ctrl Pts',(-1.36127834356734,-0.266264900654909,
0.920778333482565));
#9356=CARTESIAN_POINT('Ctrl Pts',(-1.33211611256184,-0.317195968905306,
0.962485392528369));
#9357=CARTESIAN_POINT('Ctrl Pts',(-1.31521005565926,-0.339090930684651,
0.985600426557816));
#9358=CARTESIAN_POINT('Ctrl Pts',(-1.27866649102984,-0.373586846396559,
1.03253285680459));
#9359=CARTESIAN_POINT('Ctrl Pts',(-1.25722555095714,-0.388086240756494,
1.05871835910697));
#9360=CARTESIAN_POINT('Ctrl Pts',(-1.2107812086231,-0.407068917407805,1.11153475808518));
#9361=CARTESIAN_POINT('Ctrl Pts',(-1.18575674747573,-0.411552957311693,
1.13814686046673));
#9362=CARTESIAN_POINT('Ctrl Pts',(-1.13814686046673,-0.411552957311693,
1.18575674747573));
#9363=CARTESIAN_POINT('Ctrl Pts',(-1.11153475808518,-0.407068917407805,
1.2107812086231));
#9364=CARTESIAN_POINT('Ctrl Pts',(-1.05871835910697,-0.388086240756494,
1.25722555095714));
#9365=CARTESIAN_POINT('Ctrl Pts',(-1.03253285680459,-0.373586846396559,
1.27866649102984));
#9366=CARTESIAN_POINT('Ctrl Pts',(-0.985600426557816,-0.33909093068465,
1.31521005565926));
#9367=CARTESIAN_POINT('Ctrl Pts',(-0.962485392528369,-0.317195968905306,
1.33211611256184));
#9368=CARTESIAN_POINT('Ctrl Pts',(-0.920778333482565,-0.266264900654908,
1.36127834356734));
#9369=CARTESIAN_POINT('Ctrl Pts',(-0.902193646979983,-0.237231147975234,
1.3735491215176));
#9370=CARTESIAN_POINT('Ctrl Pts',(-0.867957148219442,-0.166543350814306,
1.39550172959303));
#9371=CARTESIAN_POINT('Ctrl Pts',(-0.854205272175555,-0.123401821157026,
1.40380622184538));
#9372=CARTESIAN_POINT('Ctrl Pts',(-0.846804978391753,-0.0793800000000001,
1.40825612658882));
#9373=CARTESIAN_POINT('Origin',(-1.18440385848747,-0.07938,1.18440385848747));
#9374=CARTESIAN_POINT('Origin',(0.,-0.07938,0.));
#9375=CARTESIAN_POINT('',(-1.59456899932179,-0.07938,0.397005914195118));
#9376=CARTESIAN_POINT('Origin',(0.,-0.07938,0.));
#9377=CARTESIAN_POINT('Origin',(-1.675,-0.07938,-2.22044604925031E-16));
#9378=CARTESIAN_POINT('Origin',(-1.675,0.,-2.22044604925031E-16));
#9379=CARTESIAN_POINT('',(-1.59456899932179,-0.07938,-0.397005914195118));
#9380=CARTESIAN_POINT('',(-1.643248,-0.411552957311693,3.47540551556327E-18));
#9381=CARTESIAN_POINT('Ctrl Pts',(-1.59456899932179,-0.0793800000000001,
-0.397005914195119));
#9382=CARTESIAN_POINT('Ctrl Pts',(-1.59665523941937,-0.123401821157026,
-0.388626558458099));
#9383=CARTESIAN_POINT('Ctrl Pts',(-1.60050712143809,-0.166543350814306,
-0.373030350867485));
#9384=CARTESIAN_POINT('Ctrl Pts',(-1.60919314384089,-0.237231147975234,
-0.333298652394954));
#9385=CARTESIAN_POINT('Ctrl Pts',(-1.61365775139403,-0.266264900654909,
-0.311480544243686));
#9386=CARTESIAN_POINT('Ctrl Pts',(-1.62252828437015,-0.317195968905306,
-0.261368388670537));
#9387=CARTESIAN_POINT('Ctrl Pts',(-1.62691869420078,-0.33909093068465,-0.233069203882014));
#9388=CARTESIAN_POINT('Ctrl Pts',(-1.63426473152765,-0.373586846396559,
-0.174042761838764));
#9389=CARTESIAN_POINT('Ctrl Pts',(-1.63761964365402,-0.388086240756494,
-0.140365781471549));
#9390=CARTESIAN_POINT('Ctrl Pts',(-1.64212536811722,-0.407068917407805,
-0.0701778381840614));
#9391=CARTESIAN_POINT('Ctrl Pts',(-1.643248,-0.411552957311693,-0.0336652739555917));
#9392=CARTESIAN_POINT('Ctrl Pts',(-1.643248,-0.411552957311693,-2.0122792321331E-16));
#9393=CARTESIAN_POINT('Origin',(-1.675,-0.07938,-2.22044604925031E-16));
#9394=CARTESIAN_POINT('Ctrl Pts',(-1.643248,-0.411552957311693,-1.94289029309402E-16));
#9395=CARTESIAN_POINT('Ctrl Pts',(-1.643248,-0.411552957311693,0.0336652739555913));
#9396=CARTESIAN_POINT('Ctrl Pts',(-1.64212536811722,-0.407068917407805,
0.0701778381840609));
#9397=CARTESIAN_POINT('Ctrl Pts',(-1.63761964365402,-0.388086240756494,
0.140365781471549));
#9398=CARTESIAN_POINT('Ctrl Pts',(-1.63426473152765,-0.373586846396559,
0.174042761838763));
#9399=CARTESIAN_POINT('Ctrl Pts',(-1.62691869420078,-0.33909093068465,0.233069203882014));
#9400=CARTESIAN_POINT('Ctrl Pts',(-1.62252828437015,-0.317195968905306,
0.261368388670536));
#9401=CARTESIAN_POINT('Ctrl Pts',(-1.61365775139403,-0.266264900654909,
0.311480544243686));
#9402=CARTESIAN_POINT('Ctrl Pts',(-1.60919314384089,-0.237231147975235,
0.333298652394954));
#9403=CARTESIAN_POINT('Ctrl Pts',(-1.60050712143809,-0.166543350814306,
0.373030350867484));
#9404=CARTESIAN_POINT('Ctrl Pts',(-1.59665523941937,-0.123401821157026,
0.388626558458099));
#9405=CARTESIAN_POINT('Ctrl Pts',(-1.59456899932179,-0.0793800000000001,
0.397005914195118));
#9406=CARTESIAN_POINT('Origin',(0.,-0.07938,0.));
#9407=CARTESIAN_POINT('',(-1.40825612658882,-0.07938,-0.846804978391753));
#9408=CARTESIAN_POINT('Origin',(0.,-0.07938,0.));
#9409=CARTESIAN_POINT('Origin',(-1.18440385848747,-0.07938,-1.18440385848747));
#9410=CARTESIAN_POINT('Origin',(-1.18440385848747,0.,-1.18440385848747));
#9411=CARTESIAN_POINT('',(-0.846804978391753,-0.07938,-1.40825612658882));
#9412=CARTESIAN_POINT('Ctrl Pts',(-0.846804978391753,-0.0793800000000001,
-1.40825612658882));
#9413=CARTESIAN_POINT('Ctrl Pts',(-0.854205272175555,-0.123401821157026,
-1.40380622184538));
#9414=CARTESIAN_POINT('Ctrl Pts',(-0.867957148219442,-0.166543350814306,
-1.39550172959303));
#9415=CARTESIAN_POINT('Ctrl Pts',(-0.902193646979982,-0.237231147975234,
-1.3735491215176));
#9416=CARTESIAN_POINT('Ctrl Pts',(-0.920778333482564,-0.266264900654908,
-1.36127834356734));
#9417=CARTESIAN_POINT('Ctrl Pts',(-0.962485392528368,-0.317195968905306,
-1.33211611256184));
#9418=CARTESIAN_POINT('Ctrl Pts',(-0.985600426557816,-0.33909093068465,
-1.31521005565926));
#9419=CARTESIAN_POINT('Ctrl Pts',(-1.03253285680459,-0.373586846396559,
-1.27866649102984));
#9420=CARTESIAN_POINT('Ctrl Pts',(-1.05871835910697,-0.388086240756494,
-1.25722555095714));
#9421=CARTESIAN_POINT('Ctrl Pts',(-1.11153475808518,-0.407068917407805,
-1.2107812086231));
#9422=CARTESIAN_POINT('Ctrl Pts',(-1.13814686046673,-0.411552957311693,
-1.18575674747573));
#9423=CARTESIAN_POINT('Ctrl Pts',(-1.18575674747573,-0.411552957311693,
-1.13814686046673));
#9424=CARTESIAN_POINT('Ctrl Pts',(-1.2107812086231,-0.407068917407805,-1.11153475808518));
#9425=CARTESIAN_POINT('Ctrl Pts',(-1.25722555095714,-0.388086240756494,
-1.05871835910697));
#9426=CARTESIAN_POINT('Ctrl Pts',(-1.27866649102984,-0.373586846396559,
-1.03253285680459));
#9427=CARTESIAN_POINT('Ctrl Pts',(-1.31521005565926,-0.33909093068465,-0.985600426557816));
#9428=CARTESIAN_POINT('Ctrl Pts',(-1.33211611256184,-0.317195968905306,
-0.962485392528369));
#9429=CARTESIAN_POINT('Ctrl Pts',(-1.36127834356734,-0.266264900654909,
-0.920778333482565));
#9430=CARTESIAN_POINT('Ctrl Pts',(-1.3735491215176,-0.237231147975234,-0.902193646979983));
#9431=CARTESIAN_POINT('Ctrl Pts',(-1.39550172959303,-0.166543350814306,
-0.867957148219442));
#9432=CARTESIAN_POINT('Ctrl Pts',(-1.40380622184538,-0.123401821157026,
-0.854205272175555));
#9433=CARTESIAN_POINT('Ctrl Pts',(-1.40825612658882,-0.07938,-0.846804978391753));
#9434=CARTESIAN_POINT('Origin',(-1.18440385848747,-0.07938,-1.18440385848747));
#9435=CARTESIAN_POINT('Origin',(0.,-0.07938,0.));
#9436=CARTESIAN_POINT('',(-0.397005914195118,-0.07938,-1.59456899932179));
#9437=CARTESIAN_POINT('Origin',(0.,-0.07938,0.));
#9438=CARTESIAN_POINT('Origin',(1.11022302462516E-16,-0.07938,-1.675));
#9439=CARTESIAN_POINT('Origin',(1.11022302462516E-16,0.,-1.675));
#9440=CARTESIAN_POINT('',(0.397005914195118,-0.07938,-1.59456899932179));
#9441=CARTESIAN_POINT('Ctrl Pts',(0.397005914195119,-0.0793800000000001,
-1.59456899932179));
#9442=CARTESIAN_POINT('Ctrl Pts',(0.388626558458099,-0.123401821157026,
-1.59665523941937));
#9443=CARTESIAN_POINT('Ctrl Pts',(0.373030350867485,-0.166543350814306,
-1.60050712143809));
#9444=CARTESIAN_POINT('Ctrl Pts',(0.333298652394954,-0.237231147975234,
-1.60919314384089));
#9445=CARTESIAN_POINT('Ctrl Pts',(0.311480544243686,-0.266264900654909,
-1.61365775139403));
#9446=CARTESIAN_POINT('Ctrl Pts',(0.261368388670537,-0.317195968905306,
-1.62252828437015));
#9447=CARTESIAN_POINT('Ctrl Pts',(0.233069203882014,-0.33909093068465,-1.62691869420078));
#9448=CARTESIAN_POINT('Ctrl Pts',(0.174042761838763,-0.373586846396559,
-1.63426473152765));
#9449=CARTESIAN_POINT('Ctrl Pts',(0.140365781471549,-0.388086240756494,
-1.63761964365402));
#9450=CARTESIAN_POINT('Ctrl Pts',(0.0701778381840612,-0.407068917407805,
-1.64212536811722));
#9451=CARTESIAN_POINT('Ctrl Pts',(0.0336652739555916,-0.411552957311693,
-1.643248));
#9452=CARTESIAN_POINT('Ctrl Pts',(-0.0336652739555915,-0.411552957311693,
-1.643248));
#9453=CARTESIAN_POINT('Ctrl Pts',(-0.0701778381840612,-0.407068917407805,
-1.64212536811722));
#9454=CARTESIAN_POINT('Ctrl Pts',(-0.140365781471549,-0.388086240756494,
-1.63761964365402));
#9455=CARTESIAN_POINT('Ctrl Pts',(-0.174042761838764,-0.373586846396559,
-1.63426473152765));
#9456=CARTESIAN_POINT('Ctrl Pts',(-0.233069203882014,-0.33909093068465,
-1.62691869420078));
#9457=CARTESIAN_POINT('Ctrl Pts',(-0.261368388670536,-0.317195968905306,
-1.62252828437015));
#9458=CARTESIAN_POINT('Ctrl Pts',(-0.311480544243686,-0.266264900654908,
-1.61365775139403));
#9459=CARTESIAN_POINT('Ctrl Pts',(-0.333298652394954,-0.237231147975234,
-1.60919314384089));
#9460=CARTESIAN_POINT('Ctrl Pts',(-0.373030350867485,-0.166543350814306,
-1.60050712143809));
#9461=CARTESIAN_POINT('Ctrl Pts',(-0.388626558458099,-0.123401821157026,
-1.59665523941937));
#9462=CARTESIAN_POINT('Ctrl Pts',(-0.397005914195118,-0.07938,-1.59456899932179));
#9463=CARTESIAN_POINT('Origin',(1.11022302462516E-16,-0.07938,-1.675));
#9464=CARTESIAN_POINT('Origin',(0.,-0.07938,0.));
#9465=CARTESIAN_POINT('',(0.846804978391753,-0.07938,-1.40825612658882));
#9466=CARTESIAN_POINT('Origin',(0.,-0.07938,0.));
#9467=CARTESIAN_POINT('Origin',(1.18440385848747,-0.07938,-1.18440385848747));
#9468=CARTESIAN_POINT('Origin',(1.18440385848747,0.,-1.18440385848747));
#9469=CARTESIAN_POINT('',(1.40825612658882,-0.07938,-0.846804978391753));
#9470=CARTESIAN_POINT('Ctrl Pts',(1.40825612658882,-0.0793800000000001,
-0.846804978391753));
#9471=CARTESIAN_POINT('Ctrl Pts',(1.40380622184538,-0.123401821157026,-0.854205272175555));
#9472=CARTESIAN_POINT('Ctrl Pts',(1.39550172959303,-0.166543350814306,-0.867957148219442));
#9473=CARTESIAN_POINT('Ctrl Pts',(1.3735491215176,-0.237231147975234,-0.902193646979983));
#9474=CARTESIAN_POINT('Ctrl Pts',(1.36127834356734,-0.266264900654908,-0.920778333482565));
#9475=CARTESIAN_POINT('Ctrl Pts',(1.33211611256184,-0.317195968905306,-0.962485392528369));
#9476=CARTESIAN_POINT('Ctrl Pts',(1.31521005565926,-0.33909093068465,-0.985600426557816));
#9477=CARTESIAN_POINT('Ctrl Pts',(1.27866649102984,-0.373586846396559,-1.03253285680459));
#9478=CARTESIAN_POINT('Ctrl Pts',(1.25722555095714,-0.388086240756494,-1.05871835910697));
#9479=CARTESIAN_POINT('Ctrl Pts',(1.2107812086231,-0.407068917407805,-1.11153475808518));
#9480=CARTESIAN_POINT('Ctrl Pts',(1.18575674747573,-0.411552957311693,-1.13814686046673));
#9481=CARTESIAN_POINT('Ctrl Pts',(1.13814686046673,-0.411552957311693,-1.18575674747573));
#9482=CARTESIAN_POINT('Ctrl Pts',(1.11153475808518,-0.407068917407805,-1.2107812086231));
#9483=CARTESIAN_POINT('Ctrl Pts',(1.05871835910697,-0.388086240756494,-1.25722555095714));
#9484=CARTESIAN_POINT('Ctrl Pts',(1.03253285680459,-0.373586846396559,-1.27866649102984));
#9485=CARTESIAN_POINT('Ctrl Pts',(0.985600426557816,-0.33909093068465,-1.31521005565926));
#9486=CARTESIAN_POINT('Ctrl Pts',(0.962485392528369,-0.317195968905306,
-1.33211611256184));
#9487=CARTESIAN_POINT('Ctrl Pts',(0.920778333482565,-0.266264900654909,
-1.36127834356734));
#9488=CARTESIAN_POINT('Ctrl Pts',(0.902193646979983,-0.237231147975234,
-1.3735491215176));
#9489=CARTESIAN_POINT('Ctrl Pts',(0.867957148219442,-0.166543350814306,
-1.39550172959303));
#9490=CARTESIAN_POINT('Ctrl Pts',(0.854205272175555,-0.123401821157026,
-1.40380622184538));
#9491=CARTESIAN_POINT('Ctrl Pts',(0.846804978391753,-0.0793800000000001,
-1.40825612658882));
#9492=CARTESIAN_POINT('Origin',(1.18440385848747,-0.07938,-1.18440385848747));
#9493=CARTESIAN_POINT('Origin',(0.,-0.27783,0.));
#9494=CARTESIAN_POINT('',(-1.643248,-0.47628,2.01239840340529E-16));
#9495=CARTESIAN_POINT('Origin',(0.,-0.47628,0.));
#9496=CARTESIAN_POINT('',(-1.643248,-0.27783,2.01239840340529E-16));
#9497=CARTESIAN_POINT('',(1.59456899932179,-0.07938,0.397005914195118));
#9498=CARTESIAN_POINT('Origin',(0.,-0.07938,0.));
#9499=CARTESIAN_POINT('',(1.59456899932179,-0.07938,-0.397005914195118));
#9500=CARTESIAN_POINT('Ctrl Pts',(1.59456899932179,-0.0793800000000001,
0.397005914195118));
#9501=CARTESIAN_POINT('Ctrl Pts',(1.59665523941937,-0.123401821157026,0.388626558458099));
#9502=CARTESIAN_POINT('Ctrl Pts',(1.60050712143809,-0.166543350814306,0.373030350867485));
#9503=CARTESIAN_POINT('Ctrl Pts',(1.60919314384089,-0.237231147975234,0.333298652394954));
#9504=CARTESIAN_POINT('Ctrl Pts',(1.61365775139403,-0.266264900654909,0.311480544243686));
#9505=CARTESIAN_POINT('Ctrl Pts',(1.62252828437015,-0.317195968905306,0.261368388670537));
#9506=CARTESIAN_POINT('Ctrl Pts',(1.62691869420078,-0.33909093068465,0.233069203882014));
#9507=CARTESIAN_POINT('Ctrl Pts',(1.63426473152765,-0.373586846396559,0.174042761838764));
#9508=CARTESIAN_POINT('Ctrl Pts',(1.63761964365402,-0.388086240756494,0.140365781471549));
#9509=CARTESIAN_POINT('Ctrl Pts',(1.64212536811722,-0.407068917407805,0.0701778381840612));
#9510=CARTESIAN_POINT('Ctrl Pts',(1.643248,-0.411552957311693,0.0336652739555916));
#9511=CARTESIAN_POINT('Ctrl Pts',(1.643248,-0.411552957311693,-0.0336652739555916));
#9512=CARTESIAN_POINT('Ctrl Pts',(1.64212536811722,-0.407068917407805,-0.0701778381840612));
#9513=CARTESIAN_POINT('Ctrl Pts',(1.63761964365402,-0.388086240756494,-0.140365781471549));
#9514=CARTESIAN_POINT('Ctrl Pts',(1.63426473152765,-0.373586846396559,-0.174042761838764));
#9515=CARTESIAN_POINT('Ctrl Pts',(1.62691869420078,-0.33909093068465,-0.233069203882014));
#9516=CARTESIAN_POINT('Ctrl Pts',(1.62252828437015,-0.317195968905306,-0.261368388670537));
#9517=CARTESIAN_POINT('Ctrl Pts',(1.61365775139403,-0.266264900654909,-0.311480544243686));
#9518=CARTESIAN_POINT('Ctrl Pts',(1.60919314384089,-0.237231147975234,-0.333298652394954));
#9519=CARTESIAN_POINT('Ctrl Pts',(1.60050712143809,-0.166543350814306,-0.373030350867485));
#9520=CARTESIAN_POINT('Ctrl Pts',(1.59665523941937,-0.123401821157026,-0.388626558458099));
#9521=CARTESIAN_POINT('Ctrl Pts',(1.59456899932179,-0.07938,-0.397005914195118));
#9522=CARTESIAN_POINT('Origin',(0.,-0.07938,0.));
#9523=CARTESIAN_POINT('Origin',(0.,-0.07938,0.));
#9524=CARTESIAN_POINT('Origin',(1.675,-0.07938,0.));
#9525=CARTESIAN_POINT('Origin',(1.675,0.,0.));
#9526=CARTESIAN_POINT('Origin',(1.675,-0.07938,0.));
#9527=CARTESIAN_POINT('Origin',(0.,-0.47628,0.));
#9528=CARTESIAN_POINT('Origin',(0.,-0.07938,0.));
#9529=CARTESIAN_POINT('',(0.,0.,0.));
#9530=CARTESIAN_POINT('Origin',(1.70469,0.695,0.));
#9531=CARTESIAN_POINT('',(-1.70469,0.695,-2.0876431520385E-16));
#9532=CARTESIAN_POINT('Origin',(0.,0.695,0.));
#9533=CARTESIAN_POINT('',(-1.65031,0.695,-2.02104685910087E-16));
#9534=CARTESIAN_POINT('Origin',(0.,0.695,0.));
#9535=CARTESIAN_POINT('Origin',(0.,0.6575,0.));
#9536=CARTESIAN_POINT('',(-1.70469,0.62,-2.0876431520385E-16));
#9537=CARTESIAN_POINT('Origin',(0.,0.62,0.));
#9538=CARTESIAN_POINT('',(-1.70469,0.6575,-2.0876431520385E-16));
#9539=CARTESIAN_POINT('Origin',(1.65031,0.62,0.));
#9540=CARTESIAN_POINT('',(-1.65031,0.62,-2.02104685910087E-16));
#9541=CARTESIAN_POINT('Origin',(0.,0.62,0.));
#9542=CARTESIAN_POINT('Origin',(0.,0.6575,0.));
#9543=CARTESIAN_POINT('',(-1.65031,0.6575,-2.02104685910087E-16));
#9544=CARTESIAN_POINT('Origin',(1.70469,-0.62,0.));
#9545=CARTESIAN_POINT('',(-1.70469,-0.62,-2.0876431520385E-16));
#9546=CARTESIAN_POINT('Origin',(0.,-0.62,0.));
#9547=CARTESIAN_POINT('',(-1.65031,-0.62,-2.02104685910087E-16));
#9548=CARTESIAN_POINT('Origin',(0.,-0.62,0.));
#9549=CARTESIAN_POINT('Origin',(0.,-0.6575,0.));
#9550=CARTESIAN_POINT('',(-1.70469,-0.695,-2.0876431520385E-16));
#9551=CARTESIAN_POINT('Origin',(0.,-0.695,0.));
#9552=CARTESIAN_POINT('',(-1.70469,-0.6575,-2.0876431520385E-16));
#9553=CARTESIAN_POINT('Origin',(1.65031,-0.695,0.));
#9554=CARTESIAN_POINT('',(-1.65031,-0.695,-2.02104685910087E-16));
#9555=CARTESIAN_POINT('Origin',(0.,-0.695,0.));
#9556=CARTESIAN_POINT('Origin',(0.,-0.6575,0.));
#9557=CARTESIAN_POINT('',(-1.65031,-0.6575,-2.02104685910087E-16));
#9558=CARTESIAN_POINT('',(0.,0.,0.));
#9559=CARTESIAN_POINT('',(0.,0.,0.));
#9560=CARTESIAN_POINT('',(0.,0.,0.));
#9561=CARTESIAN_POINT('',(0.,0.,0.));
#9562=CARTESIAN_POINT('',(0.,0.,0.));
#9563=CARTESIAN_POINT('',(0.,0.,0.));
#9564=CARTESIAN_POINT('Origin',(0.45,0.6,0.));
#9565=CARTESIAN_POINT('',(-0.45,0.6,-5.51091059616309E-17));
#9566=CARTESIAN_POINT('Origin',(0.,0.6,0.));
#9567=CARTESIAN_POINT('Origin',(0.,0.575,0.));
#9568=CARTESIAN_POINT('',(-0.5,0.55,-6.12323399573677E-17));
#9569=CARTESIAN_POINT('Origin',(0.,0.55,0.));
#9570=CARTESIAN_POINT('',(-0.475,0.575,-5.81707229594993E-17));
#9571=CARTESIAN_POINT('Origin',(0.,0.29,0.));
#9572=CARTESIAN_POINT('',(-0.5,0.0299999999999998,-6.12323399573677E-17));
#9573=CARTESIAN_POINT('Origin',(0.,0.0299999999999998,0.));
#9574=CARTESIAN_POINT('',(-0.5,0.29,-6.12323399573677E-17));
#9575=CARTESIAN_POINT('Origin',(0.,0.0150000000000001,0.));
#9576=CARTESIAN_POINT('',(-0.47,7.11236625150491E-17,-5.75583995599256E-17));
#9577=CARTESIAN_POINT('Origin',(0.,0.,0.));
#9578=CARTESIAN_POINT('',(-0.485,0.0150000000000001,-5.93953697586466E-17));
#9579=CARTESIAN_POINT('Origin',(0.32,0.,0.));
#9580=CARTESIAN_POINT('',(-0.32,-6.93889390390723E-18,-3.91886975727153E-17));
#9581=CARTESIAN_POINT('Origin',(0.,0.,0.));
#9582=CARTESIAN_POINT('Origin',(0.,-0.02,0.));
#9583=CARTESIAN_POINT('',(-0.2942,-0.0515999999999999,3.60291088309151E-17));
#9584=CARTESIAN_POINT('Origin',(0.,-0.0515999999999999,0.));
#9585=CARTESIAN_POINT('',(-0.31,-0.02,-3.7964050773568E-17));
#9586=CARTESIAN_POINT('Origin',(0.,-1.24,0.));
#9587=CARTESIAN_POINT('',(-0.2942,-2.4458,3.60291088309151E-17));
#9588=CARTESIAN_POINT('Origin',(0.,-2.4458,0.));
#9589=CARTESIAN_POINT('',(-0.2942,-1.24,-3.60291088309151E-17));
#9590=CARTESIAN_POINT('Origin',(0.,-2.47,0.));
#9591=CARTESIAN_POINT('',(-0.24,-2.5,-2.93915231795365E-17));
#9592=CARTESIAN_POINT('Origin',(0.,-2.5,0.));
#9593=CARTESIAN_POINT('',(-0.27,-2.47,-3.30654635769785E-17));
#9594=CARTESIAN_POINT('Origin',(0.,-2.5,0.));
#9595=CARTESIAN_POINT('Origin',(0.144337567297406,-0.6,-0.25));
#9596=CARTESIAN_POINT('',(0.288675134594813,-0.6,0.));
#9597=CARTESIAN_POINT('',(0.144337567297406,-0.6,-0.25));
#9598=CARTESIAN_POINT('',(0.288675134594813,-0.6,0.));
#9599=CARTESIAN_POINT('',(0.144337567297406,-0.96,-0.25));
#9600=CARTESIAN_POINT('',(0.144337567297406,-0.6,-0.25));
#9601=CARTESIAN_POINT('',(0.288675134594813,-0.96,0.));
#9602=CARTESIAN_POINT('',(0.288675134594813,-0.96,0.));
#9603=CARTESIAN_POINT('',(0.288675134594813,-0.6,0.));
#9604=CARTESIAN_POINT('Origin',(-0.144337567297406,-0.6,-0.25));
#9605=CARTESIAN_POINT('',(-0.144337567297406,-0.6,-0.25));
#9606=CARTESIAN_POINT('',(0.144337567297406,-0.6,-0.25));
#9607=CARTESIAN_POINT('',(-0.144337567297406,-0.96,-0.25));
#9608=CARTESIAN_POINT('',(-0.144337567297406,-0.6,-0.25));
#9609=CARTESIAN_POINT('',(0.144337567297406,-0.96,-0.25));
#9610=CARTESIAN_POINT('Origin',(-0.288675134594813,-0.6,-8.32667268468867E-17));
#9611=CARTESIAN_POINT('',(-0.288675134594813,-0.6,-3.53525079574969E-17));
#9612=CARTESIAN_POINT('',(-0.144337567297406,-0.6,-0.25));
#9613=CARTESIAN_POINT('',(-0.288675134594813,-0.96,-5.55111512312578E-17));
#9614=CARTESIAN_POINT('',(-0.288675134594813,-0.6,-3.53525079574969E-17));
#9615=CARTESIAN_POINT('',(-0.144337567297406,-0.96,-0.25));
#9616=CARTESIAN_POINT('Origin',(-0.144337567297407,-0.6,0.25));
#9617=CARTESIAN_POINT('',(-0.144337567297407,-0.6,0.25));
#9618=CARTESIAN_POINT('',(-0.288675134594813,-0.6,-3.53525079574969E-17));
#9619=CARTESIAN_POINT('',(-0.144337567297407,-0.96,0.25));
#9620=CARTESIAN_POINT('',(-0.144337567297407,-0.6,0.25));
#9621=CARTESIAN_POINT('',(-0.288675134594813,-0.96,-3.53525079574969E-17));
#9622=CARTESIAN_POINT('Origin',(0.144337567297406,-0.6,0.25));
#9623=CARTESIAN_POINT('',(0.144337567297406,-0.6,0.25));
#9624=CARTESIAN_POINT('',(-0.144337567297407,-0.6,0.25));
#9625=CARTESIAN_POINT('',(0.144337567297406,-0.96,0.25));
#9626=CARTESIAN_POINT('',(0.144337567297406,-0.6,0.25));
#9627=CARTESIAN_POINT('',(-0.144337567297407,-0.96,0.25));
#9628=CARTESIAN_POINT('Origin',(0.288675134594813,-0.6,0.));
#9629=CARTESIAN_POINT('',(0.144337567297406,-0.6,0.25));
#9630=CARTESIAN_POINT('',(0.144337567297406,-0.96,0.25));
#9631=CARTESIAN_POINT('Origin',(0.,-0.6,0.));
#9632=CARTESIAN_POINT('Origin',(0.,-0.96,0.));
#9633=CARTESIAN_POINT('',(0.,0.,0.));
#9634=CARTESIAN_POINT('Origin',(0.3,0.4,0.));
#9635=CARTESIAN_POINT('',(-0.3,0.4,-3.67394039744206E-17));
#9636=CARTESIAN_POINT('Origin',(0.,0.4,0.));
#9637=CARTESIAN_POINT('Origin',(0.,0.375,0.));
#9638=CARTESIAN_POINT('',(-0.35,0.35,-4.28626379701573E-17));
#9639=CARTESIAN_POINT('Origin',(0.,0.35,0.));
#9640=CARTESIAN_POINT('',(-0.325,0.375,-3.9801020972289E-17));
#9641=CARTESIAN_POINT('Origin',(0.,0.19,0.));
#9642=CARTESIAN_POINT('',(-0.35,0.03,-4.28626379701574E-17));
#9643=CARTESIAN_POINT('Origin',(0.,0.03,0.));
#9644=CARTESIAN_POINT('',(-0.35,0.19,-4.28626379701574E-17));
#9645=CARTESIAN_POINT('Origin',(0.,0.0149999999999999,0.));
#9646=CARTESIAN_POINT('',(-0.32,-3.29597460435593E-17,-3.91886975727153E-17));
#9647=CARTESIAN_POINT('Origin',(0.,0.,0.));
#9648=CARTESIAN_POINT('',(-0.335,0.0149999999999999,-4.10256677714363E-17));
#9649=CARTESIAN_POINT('Origin',(0.22,0.,0.));
#9650=CARTESIAN_POINT('',(-0.22,-6.93889390390723E-18,-2.69422295812418E-17));
#9651=CARTESIAN_POINT('Origin',(0.,0.,0.));
#9652=CARTESIAN_POINT('Origin',(0.,-0.02,0.));
#9653=CARTESIAN_POINT('',(-0.1954,-0.0492,2.39295984553393E-17));
#9654=CARTESIAN_POINT('Origin',(0.,-0.0492,0.));
#9655=CARTESIAN_POINT('',(-0.21,-0.02,-2.57175827820944E-17));
#9656=CARTESIAN_POINT('Origin',(0.,-0.8,0.));
#9657=CARTESIAN_POINT('',(-0.1954,-1.5646,2.39295984553393E-17));
#9658=CARTESIAN_POINT('Origin',(0.,-1.5646,0.));
#9659=CARTESIAN_POINT('',(-0.1954,-0.8,-2.39295984553393E-17));
#9660=CARTESIAN_POINT('Origin',(0.,-1.58,0.));
#9661=CARTESIAN_POINT('',(-0.16,-1.6,-1.95943487863577E-17));
#9662=CARTESIAN_POINT('Origin',(0.,-1.6,0.));
#9663=CARTESIAN_POINT('',(-0.18,-1.58,-2.20436423846524E-17));
#9664=CARTESIAN_POINT('Origin',(0.,-1.6,0.));
#9665=CARTESIAN_POINT('Origin',(0.0866025403784439,-0.4,-0.15));
#9666=CARTESIAN_POINT('',(0.173205080756888,-0.4,0.));
#9667=CARTESIAN_POINT('',(0.0866025403784439,-0.4,-0.15));
#9668=CARTESIAN_POINT('',(0.173205080756888,-0.4,0.));
#9669=CARTESIAN_POINT('',(0.0866025403784439,-0.64,-0.15));
#9670=CARTESIAN_POINT('',(0.0866025403784439,-0.4,-0.15));
#9671=CARTESIAN_POINT('',(0.173205080756888,-0.64,0.));
#9672=CARTESIAN_POINT('',(0.173205080756888,-0.64,0.));
#9673=CARTESIAN_POINT('',(0.173205080756888,-0.4,0.));
#9674=CARTESIAN_POINT('Origin',(-0.0866025403784438,-0.4,-0.15));
#9675=CARTESIAN_POINT('',(-0.0866025403784438,-0.4,-0.15));
#9676=CARTESIAN_POINT('',(0.0866025403784439,-0.4,-0.15));
#9677=CARTESIAN_POINT('',(-0.0866025403784438,-0.64,-0.15));
#9678=CARTESIAN_POINT('',(-0.0866025403784438,-0.4,-0.15));
#9679=CARTESIAN_POINT('',(0.0866025403784439,-0.64,-0.15));
#9680=CARTESIAN_POINT('Origin',(-0.173205080756888,-0.4,-2.77555756156289E-17));
#9681=CARTESIAN_POINT('',(-0.173205080756888,-0.4,-2.12115047744981E-17));
#9682=CARTESIAN_POINT('',(-0.0866025403784438,-0.4,-0.15));
#9683=CARTESIAN_POINT('',(-0.173205080756888,-0.64,-2.77555756156289E-17));
#9684=CARTESIAN_POINT('',(-0.173205080756888,-0.4,-2.12115047744981E-17));
#9685=CARTESIAN_POINT('',(-0.0866025403784438,-0.64,-0.15));
#9686=CARTESIAN_POINT('Origin',(-0.0866025403784439,-0.4,0.15));
#9687=CARTESIAN_POINT('',(-0.0866025403784439,-0.4,0.15));
#9688=CARTESIAN_POINT('',(-0.173205080756888,-0.4,-2.12115047744981E-17));
#9689=CARTESIAN_POINT('',(-0.0866025403784439,-0.64,0.15));
#9690=CARTESIAN_POINT('',(-0.0866025403784439,-0.4,0.15));
#9691=CARTESIAN_POINT('',(-0.173205080756888,-0.64,-2.12115047744981E-17));
#9692=CARTESIAN_POINT('Origin',(0.0866025403784439,-0.4,0.15));
#9693=CARTESIAN_POINT('',(0.0866025403784439,-0.4,0.15));
#9694=CARTESIAN_POINT('',(-0.0866025403784439,-0.4,0.15));
#9695=CARTESIAN_POINT('',(0.0866025403784439,-0.64,0.15));
#9696=CARTESIAN_POINT('',(0.0866025403784439,-0.4,0.15));
#9697=CARTESIAN_POINT('',(-0.0866025403784439,-0.64,0.15));
#9698=CARTESIAN_POINT('Origin',(0.173205080756888,-0.4,0.));
#9699=CARTESIAN_POINT('',(0.0866025403784439,-0.4,0.15));
#9700=CARTESIAN_POINT('',(0.0866025403784439,-0.64,0.15));
#9701=CARTESIAN_POINT('Origin',(0.,-0.4,-2.77555756156289E-17));
#9702=CARTESIAN_POINT('Origin',(0.,-0.64,-2.77555756156289E-17));
#9703=CARTESIAN_POINT('',(0.,0.,0.));
#9704=CARTESIAN_POINT('',(0.,0.,0.));
#9705=CARTESIAN_POINT('',(0.,0.,0.));
#9706=CARTESIAN_POINT('',(0.,0.,0.));
#9707=CARTESIAN_POINT('',(0.,0.,0.));
#9708=CARTESIAN_POINT('',(0.,0.,0.));
#9709=CARTESIAN_POINT('',(0.,0.,0.));
#9710=CARTESIAN_POINT('',(0.,0.,0.));
#9711=CARTESIAN_POINT('',(0.,1.,4.5));
#9712=CARTESIAN_POINT('',(-3.8,1.,2.5));
#9713=CARTESIAN_POINT('',(3.8,1.,2.5));
#9714=CARTESIAN_POINT('',(0.,5.,4.5));
#9715=CARTESIAN_POINT('',(-3.8,5.,2.5));
#9716=CARTESIAN_POINT('',(3.8,5.,2.5));
#9717=CARTESIAN_POINT('',(2.8,-0.4,4.5));
#9718=CARTESIAN_POINT('',(0.,-0.4,7.3));
#9719=CARTESIAN_POINT('',(-2.8,-0.4,4.5));
#9720=CARTESIAN_POINT('',(-4.44089209850063E-16,-0.4,1.7));
#9721=CARTESIAN_POINT('',(2.8,6.4,4.5));
#9722=CARTESIAN_POINT('',(4.44089209850063E-16,6.4,7.3));
#9723=CARTESIAN_POINT('',(-2.8,6.4,4.5));
#9724=CARTESIAN_POINT('',(-4.44089209850063E-16,6.4,1.7));
#9725=CARTESIAN_POINT('',(0.,0.,0.));
#9726=CARTESIAN_POINT('',(0.,0.,0.));
#9727=CARTESIAN_POINT('Origin',(-0.2,8.15,3.8));
#9728=CARTESIAN_POINT('',(-0.2,9.6,3.93431457505076));
#9729=CARTESIAN_POINT('',(-0.2,8.15,3.93431457505076));
#9730=CARTESIAN_POINT('',(-0.2,8.,3.93431457505076));
#9731=CARTESIAN_POINT('',(-0.2,9.6,4.15));
#9732=CARTESIAN_POINT('',(-0.2,9.6,4.15));
#9733=CARTESIAN_POINT('',(-0.2,8.15,4.15));
#9734=CARTESIAN_POINT('',(-0.2,8.15,4.15));
#9735=CARTESIAN_POINT('',(-0.2,8.15,4.15));
#9736=CARTESIAN_POINT('Origin',(0.,8.15,3.975));
#9737=CARTESIAN_POINT('',(0.2,8.15,3.93431457505076));
#9738=CARTESIAN_POINT('Origin',(0.,8.15,4.5));
#9739=CARTESIAN_POINT('',(0.2,8.15,4.15));
#9740=CARTESIAN_POINT('',(0.2,8.15,4.15));
#9741=CARTESIAN_POINT('',(0.2,8.15,3.8));
#9742=CARTESIAN_POINT('Origin',(0.2,8.15,4.15));
#9743=CARTESIAN_POINT('',(0.2,9.6,3.93431457505076));
#9744=CARTESIAN_POINT('',(0.2,8.,3.93431457505076));
#9745=CARTESIAN_POINT('',(0.2,9.6,4.15));
#9746=CARTESIAN_POINT('',(0.2,8.15,4.15));
#9747=CARTESIAN_POINT('',(0.2,9.6,3.8));
#9748=CARTESIAN_POINT('Origin',(-0.2,8.15,4.15));
#9749=CARTESIAN_POINT('',(0.2,9.6,4.15));
#9750=CARTESIAN_POINT('Origin',(0.,9.6,3.975));
#9751=CARTESIAN_POINT('Origin',(0.,9.6,4.5));
#9752=CARTESIAN_POINT('Origin',(0.,8.,4.5));
#9753=CARTESIAN_POINT('',(-0.6,10.6,4.5));
#9754=CARTESIAN_POINT('Origin',(0.,10.6,4.5));
#9755=CARTESIAN_POINT('',(-0.6,8.,4.5));
#9756=CARTESIAN_POINT('',(-0.6,8.,4.5));
#9757=CARTESIAN_POINT('Origin',(0.,8.,4.5));
#9758=CARTESIAN_POINT('Origin',(0.,10.6,4.5));
#9759=CARTESIAN_POINT('Origin',(0.,0.3,4.5));
#9760=CARTESIAN_POINT('',(-1.2,0.3,4.5));
#9761=CARTESIAN_POINT('Origin',(0.,0.3,4.5));
#9762=CARTESIAN_POINT('',(-1.,0.3,4.5));
#9763=CARTESIAN_POINT('Origin',(0.,0.3,4.5));
#9764=CARTESIAN_POINT('Origin',(0.,0.,4.5));
#9765=CARTESIAN_POINT('',(-1.2,0.,4.5));
#9766=CARTESIAN_POINT('Origin',(0.,0.,4.5));
#9767=CARTESIAN_POINT('',(-1.,0.,4.5));
#9768=CARTESIAN_POINT('Origin',(0.,0.,4.5));
#9769=CARTESIAN_POINT('Origin',(0.,0.,4.5));
#9770=CARTESIAN_POINT('',(-1.2,0.,4.5));
#9771=CARTESIAN_POINT('Origin',(0.,-2.,4.5));
#9772=CARTESIAN_POINT('',(-1.,-2.,4.5));
#9773=CARTESIAN_POINT('',(-1.,-2.,4.5));
#9774=CARTESIAN_POINT('Origin',(0.,-2.,4.5));
#9775=CARTESIAN_POINT('Origin',(0.,-2.,4.5));
#9776=CARTESIAN_POINT('',(-1.,8.,4.5));
#9777=CARTESIAN_POINT('Origin',(0.,8.,4.5));
#9778=CARTESIAN_POINT('',(-1.,-2.,4.5));
#9779=CARTESIAN_POINT('Origin',(0.,8.,4.5));
#9780=CARTESIAN_POINT('Origin',(0.,-2.,4.5));
#9781=CARTESIAN_POINT('',(0.,0.,0.));
#9782=CARTESIAN_POINT('Origin',(0.,5.7,4.5));
#9783=CARTESIAN_POINT('',(-1.01,6.4,4.5));
#9784=CARTESIAN_POINT('Origin',(0.,6.4,4.5));
#9785=CARTESIAN_POINT('',(-1.01,5.7,4.5));
#9786=CARTESIAN_POINT('',(-1.01,5.7,4.5));
#9787=CARTESIAN_POINT('Origin',(0.,5.7,4.5));
#9788=CARTESIAN_POINT('Origin',(0.,5.7,4.5));
#9789=CARTESIAN_POINT('',(-1.35,6.4,4.5));
#9790=CARTESIAN_POINT('Origin',(0.,6.4,4.5));
#9791=CARTESIAN_POINT('',(-1.35,5.7,4.5));
#9792=CARTESIAN_POINT('',(-1.35,5.7,4.5));
#9793=CARTESIAN_POINT('Origin',(0.,5.7,4.5));
#9794=CARTESIAN_POINT('Origin',(0.,6.4,4.5));
#9795=CARTESIAN_POINT('Origin',(0.,5.7,4.5));
#9796=CARTESIAN_POINT('',(0.,0.,0.));
#9797=CARTESIAN_POINT('Origin',(0.,6.8,5.49));
#9798=CARTESIAN_POINT('',(0.172988438920061,6.68094119100209,5.49));
#9799=CARTESIAN_POINT('',(0.172988438920061,6.91905880899791,5.49));
#9800=CARTESIAN_POINT('',(0.172988438920061,6.4,5.49));
#9801=CARTESIAN_POINT('Origin',(0.,6.8,5.49));
#9802=CARTESIAN_POINT('Origin',(0.,6.8,5.49));
#9803=CARTESIAN_POINT('',(-0.172988438920061,6.68094119100209,5.49));
#9804=CARTESIAN_POINT('Ctrl Pts',(-0.172988438920061,6.68094119100209,5.49));
#9805=CARTESIAN_POINT('Ctrl Pts',(-0.165594865311318,6.67019857760471,5.49129192197638));
#9806=CARTESIAN_POINT('Ctrl Pts',(-0.157297138725608,6.66031229062726,5.49265394943905));
#9807=CARTESIAN_POINT('Ctrl Pts',(-0.129892073845076,6.63290722574673,5.4967480843909));
#9808=CARTESIAN_POINT('Ctrl Pts',(-0.106330167759285,6.61675794366705,5.49969589327638));
#9809=CARTESIAN_POINT('Ctrl Pts',(-0.0546129046324107,6.59530220603509,
5.50385029472357));
#9810=CARTESIAN_POINT('Ctrl Pts',(-0.0264512308298516,6.59,5.505));
#9811=CARTESIAN_POINT('Ctrl Pts',(0.0264512308298515,6.59,5.505));
#9812=CARTESIAN_POINT('Ctrl Pts',(0.0546129046324106,6.59530220603509,5.50385029472357));
#9813=CARTESIAN_POINT('Ctrl Pts',(0.106330167759285,6.61675794366705,5.49969589327638));
#9814=CARTESIAN_POINT('Ctrl Pts',(0.129892073845076,6.63290722574673,5.4967480843909));
#9815=CARTESIAN_POINT('Ctrl Pts',(0.157297138725608,6.66031229062726,5.49265394943905));
#9816=CARTESIAN_POINT('Ctrl Pts',(0.165594865311318,6.67019857760471,5.49129192197638));
#9817=CARTESIAN_POINT('Ctrl Pts',(0.172988438920061,6.68094119100209,5.49));
#9818=CARTESIAN_POINT('',(-0.21,6.8,5.49));
#9819=CARTESIAN_POINT('Origin',(0.,6.8,5.49));
#9820=CARTESIAN_POINT('',(-0.21,6.8,5.98522725533839));
#9821=CARTESIAN_POINT('',(-0.21,6.8,5.49));
#9822=CARTESIAN_POINT('',(0.21,6.8,5.98522725533839));
#9823=CARTESIAN_POINT('Ctrl Pts',(0.21,6.8,5.98522725533839));
#9824=CARTESIAN_POINT('Ctrl Pts',(0.21,6.77359447307555,5.98522725533839));
#9825=CARTESIAN_POINT('Ctrl Pts',(0.204715737269596,6.74545292590929,5.98600415954412));
#9826=CARTESIAN_POINT('Ctrl Pts',(0.183273763036331,6.69372373109487,5.98880073282317));
#9827=CARTESIAN_POINT('Ctrl Pts',(0.167117923970394,6.67013307587204,5.99077897157582));
#9828=CARTESIAN_POINT('Ctrl Pts',(0.129867169887369,6.63288232178902,5.99448481141327));
#9829=CARTESIAN_POINT('Ctrl Pts',(0.106276408305765,6.61672628999865,5.99645455657129));
#9830=CARTESIAN_POINT('Ctrl Pts',(0.0545468514059003,6.59528417517378,5.99923165515646));
#9831=CARTESIAN_POINT('Ctrl Pts',(0.0264051785092814,6.59,6.));
#9832=CARTESIAN_POINT('Ctrl Pts',(-0.0264051785092814,6.59,6.));
#9833=CARTESIAN_POINT('Ctrl Pts',(-0.0545468514059002,6.59528417517378,
5.99923165515646));
#9834=CARTESIAN_POINT('Ctrl Pts',(-0.106276408305765,6.61672628999865,5.99645455657129));
#9835=CARTESIAN_POINT('Ctrl Pts',(-0.129867169887369,6.63288232178902,5.99448481141327));
#9836=CARTESIAN_POINT('Ctrl Pts',(-0.167117923970394,6.67013307587204,5.99077897157582));
#9837=CARTESIAN_POINT('Ctrl Pts',(-0.183273763036331,6.69372373109487,5.98880073282317));
#9838=CARTESIAN_POINT('Ctrl Pts',(-0.204715737269596,6.74545292590929,5.98600415954412));
#9839=CARTESIAN_POINT('Ctrl Pts',(-0.21,6.77359447307555,5.98522725533839));
#9840=CARTESIAN_POINT('Ctrl Pts',(-0.21,6.8,5.98522725533839));
#9841=CARTESIAN_POINT('Ctrl Pts',(-0.21,6.8,5.98522725533839));
#9842=CARTESIAN_POINT('Ctrl Pts',(-0.21,6.82640552692445,5.98522725533839));
#9843=CARTESIAN_POINT('Ctrl Pts',(-0.204715737269596,6.85454707409071,5.98600415954412));
#9844=CARTESIAN_POINT('Ctrl Pts',(-0.183273763036331,6.90627626890513,5.98880073282317));
#9845=CARTESIAN_POINT('Ctrl Pts',(-0.167117923970394,6.92986692412796,5.99077897157582));
#9846=CARTESIAN_POINT('Ctrl Pts',(-0.129867169887369,6.96711767821098,5.99448481141327));
#9847=CARTESIAN_POINT('Ctrl Pts',(-0.106276408305765,6.98327371000135,5.99645455657129));
#9848=CARTESIAN_POINT('Ctrl Pts',(-0.0545468514059003,7.00471582482622,
5.99923165515646));
#9849=CARTESIAN_POINT('Ctrl Pts',(-0.0264051785092815,7.01,6.));
#9850=CARTESIAN_POINT('Ctrl Pts',(0.0264051785092814,7.01,6.));
#9851=CARTESIAN_POINT('Ctrl Pts',(0.0545468514058999,7.00471582482622,5.99923165515646));
#9852=CARTESIAN_POINT('Ctrl Pts',(0.106276408305765,6.98327371000135,5.99645455657129));
#9853=CARTESIAN_POINT('Ctrl Pts',(0.129867169887369,6.96711767821098,5.99448481141327));
#9854=CARTESIAN_POINT('Ctrl Pts',(0.167117923970393,6.92986692412796,5.99077897157582));
#9855=CARTESIAN_POINT('Ctrl Pts',(0.183273763036332,6.90627626890513,5.98880073282317));
#9856=CARTESIAN_POINT('Ctrl Pts',(0.204715737269596,6.85454707409071,5.98600415954412));
#9857=CARTESIAN_POINT('Ctrl Pts',(0.21,6.82640552692445,5.98522725533839));
#9858=CARTESIAN_POINT('Ctrl Pts',(0.21,6.8,5.98522725533839));
#9859=CARTESIAN_POINT('',(-0.172988438920061,6.91905880899791,5.49));
#9860=CARTESIAN_POINT('Origin',(0.,6.8,5.49));
#9861=CARTESIAN_POINT('Ctrl Pts',(0.172988438920062,6.91905880899791,5.49));
#9862=CARTESIAN_POINT('Ctrl Pts',(0.165594865311319,6.92980142239529,5.49129192197638));
#9863=CARTESIAN_POINT('Ctrl Pts',(0.157297138725609,6.93968770937274,5.49265394943905));
#9864=CARTESIAN_POINT('Ctrl Pts',(0.129892073845076,6.96709277425327,5.4967480843909));
#9865=CARTESIAN_POINT('Ctrl Pts',(0.106330167759285,6.98324205633295,5.49969589327638));
#9866=CARTESIAN_POINT('Ctrl Pts',(0.0546129046324107,7.00469779396491,5.50385029472357));
#9867=CARTESIAN_POINT('Ctrl Pts',(0.0264512308298516,7.01,5.505));
#9868=CARTESIAN_POINT('Ctrl Pts',(-0.0264512308298515,7.01,5.505));
#9869=CARTESIAN_POINT('Ctrl Pts',(-0.0546129046324097,7.00469779396491,
5.50385029472357));
#9870=CARTESIAN_POINT('Ctrl Pts',(-0.106330167759284,6.98324205633295,5.49969589327638));
#9871=CARTESIAN_POINT('Ctrl Pts',(-0.129892073845076,6.96709277425327,5.4967480843909));
#9872=CARTESIAN_POINT('Ctrl Pts',(-0.157297138725609,6.93968770937274,5.49265394943905));
#9873=CARTESIAN_POINT('Ctrl Pts',(-0.165594865311318,6.92980142239529,5.49129192197638));
#9874=CARTESIAN_POINT('Ctrl Pts',(-0.172988438920061,6.91905880899791,5.49));
#9875=CARTESIAN_POINT('Origin',(0.,6.8,5.49));
#9876=CARTESIAN_POINT('',(-0.172988438920061,6.4,5.49));
#9877=CARTESIAN_POINT('Origin',(0.,6.4,4.5));
#9878=CARTESIAN_POINT('',(-1.005,7.2,4.5));
#9879=CARTESIAN_POINT('Origin',(0.,7.2,4.5));
#9880=CARTESIAN_POINT('',(-1.005,6.4,4.5));
#9881=CARTESIAN_POINT('',(-1.005,6.4,4.5));
#9882=CARTESIAN_POINT('Origin',(0.,6.4,4.5));
#9883=CARTESIAN_POINT('Origin',(0.,6.4,4.5));
#9884=CARTESIAN_POINT('',(-1.5,7.2,4.5));
#9885=CARTESIAN_POINT('Origin',(0.,7.2,4.5));
#9886=CARTESIAN_POINT('',(-1.5,6.4,4.5));
#9887=CARTESIAN_POINT('',(-1.5,6.4,4.5));
#9888=CARTESIAN_POINT('Origin',(0.,6.4,4.5));
#9889=CARTESIAN_POINT('Origin',(0.,7.2,4.5));
#9890=CARTESIAN_POINT('Origin',(0.,6.4,4.5));
#9891=CARTESIAN_POINT('',(0.,0.,0.));
#9892=CARTESIAN_POINT('Origin',(0.,10.15,5.09));
#9893=CARTESIAN_POINT('',(0.133884278389959,9.98821310312637,5.09));
#9894=CARTESIAN_POINT('',(0.133884278389959,10.3117868968736,5.09));
#9895=CARTESIAN_POINT('',(0.133884278389959,9.75,5.09));
#9896=CARTESIAN_POINT('Origin',(0.,10.15,5.09));
#9897=CARTESIAN_POINT('Origin',(0.,10.15,5.09));
#9898=CARTESIAN_POINT('',(-0.133884278389959,9.98821310312637,5.09));
#9899=CARTESIAN_POINT('Ctrl Pts',(-0.13388427838996,9.98821310312637,5.09));
#9900=CARTESIAN_POINT('Ctrl Pts',(-0.118254395260805,9.97527883178237,5.09354677224418));
#9901=CARTESIAN_POINT('Ctrl Pts',(-0.1001097876823,9.96420068341256,5.09698224789957));
#9902=CARTESIAN_POINT('Ctrl Pts',(-0.054829872132519,9.94536143894557,5.1030741628997));
#9903=CARTESIAN_POINT('Ctrl Pts',(-0.0266020595922903,9.94,5.105));
#9904=CARTESIAN_POINT('Ctrl Pts',(0.0266020595922903,9.94,5.105));
#9905=CARTESIAN_POINT('Ctrl Pts',(0.0548298721325189,9.94536143894557,5.1030741628997));
#9906=CARTESIAN_POINT('Ctrl Pts',(0.1001097876823,9.96420068341256,5.09698224789957));
#9907=CARTESIAN_POINT('Ctrl Pts',(0.118254395260804,9.97527883178237,5.09354677224418));
#9908=CARTESIAN_POINT('Ctrl Pts',(0.133884278389959,9.98821310312637,5.09));
#9909=CARTESIAN_POINT('',(-0.21,10.15,5.09));
#9910=CARTESIAN_POINT('Origin',(0.,10.15,5.09));
#9911=CARTESIAN_POINT('',(-0.21,10.15,5.68148212005091));
#9912=CARTESIAN_POINT('',(-0.21,10.15,5.09));
#9913=CARTESIAN_POINT('',(0.21,10.15,5.68148212005091));
#9914=CARTESIAN_POINT('Ctrl Pts',(0.21,10.15,5.68148212005091));
#9915=CARTESIAN_POINT('Ctrl Pts',(0.21,10.1235729289857,5.68148212005091));
#9916=CARTESIAN_POINT('Ctrl Pts',(0.204707379175836,10.0954224459113,5.68246056146672));
#9917=CARTESIAN_POINT('Ctrl Pts',(0.183259409780014,10.0436994304444,5.68597389417424));
#9918=CARTESIAN_POINT('Ctrl Pts',(0.167106958412512,10.0201221103142,5.68845578531258));
#9919=CARTESIAN_POINT('Ctrl Pts',(0.129878495645339,9.98289364754699,5.6930982535617));
#9920=CARTESIAN_POINT('Ctrl Pts',(0.106300916040875,9.96674072098398,5.69556345497295));
#9921=CARTESIAN_POINT('Ctrl Pts',(0.0545770066794469,9.94529240674315,5.69903845223025));
#9922=CARTESIAN_POINT('Ctrl Pts',(0.0264262107330192,9.94,5.7));
#9923=CARTESIAN_POINT('Ctrl Pts',(-0.0264262107330192,9.94,5.7));
#9924=CARTESIAN_POINT('Ctrl Pts',(-0.0545770066794469,9.94529240674315,
5.69903845223025));
#9925=CARTESIAN_POINT('Ctrl Pts',(-0.106300916040875,9.96674072098398,5.69556345497295));
#9926=CARTESIAN_POINT('Ctrl Pts',(-0.129878495645339,9.98289364754699,5.6930982535617));
#9927=CARTESIAN_POINT('Ctrl Pts',(-0.167106958412512,10.0201221103142,5.68845578531258));
#9928=CARTESIAN_POINT('Ctrl Pts',(-0.183259409780014,10.0436994304444,5.68597389417424));
#9929=CARTESIAN_POINT('Ctrl Pts',(-0.204707379175836,10.0954224459113,5.68246056146672));
#9930=CARTESIAN_POINT('Ctrl Pts',(-0.21,10.1235729289857,5.68148212005091));
#9931=CARTESIAN_POINT('Ctrl Pts',(-0.21,10.15,5.68148212005091));
#9932=CARTESIAN_POINT('Ctrl Pts',(-0.21,10.15,5.68148212005091));
#9933=CARTESIAN_POINT('Ctrl Pts',(-0.21,10.1764270710143,5.68148212005091));
#9934=CARTESIAN_POINT('Ctrl Pts',(-0.204707379175836,10.2045775540887,5.68246056146672));
#9935=CARTESIAN_POINT('Ctrl Pts',(-0.183259409780014,10.2563005695556,5.68597389417424));
#9936=CARTESIAN_POINT('Ctrl Pts',(-0.167106958412512,10.2798778896858,5.68845578531258));
#9937=CARTESIAN_POINT('Ctrl Pts',(-0.129878495645339,10.317106352453,5.6930982535617));
#9938=CARTESIAN_POINT('Ctrl Pts',(-0.106300916040875,10.333259279016,5.69556345497295));
#9939=CARTESIAN_POINT('Ctrl Pts',(-0.0545770066794469,10.3547075932569,
5.69903845223025));
#9940=CARTESIAN_POINT('Ctrl Pts',(-0.0264262107330192,10.36,5.7));
#9941=CARTESIAN_POINT('Ctrl Pts',(0.0264262107330191,10.36,5.7));
#9942=CARTESIAN_POINT('Ctrl Pts',(0.0545770066794468,10.3547075932569,5.69903845223025));
#9943=CARTESIAN_POINT('Ctrl Pts',(0.106300916040875,10.333259279016,5.69556345497295));
#9944=CARTESIAN_POINT('Ctrl Pts',(0.129878495645339,10.317106352453,5.6930982535617));
#9945=CARTESIAN_POINT('Ctrl Pts',(0.167106958412512,10.2798778896858,5.68845578531258));
#9946=CARTESIAN_POINT('Ctrl Pts',(0.183259409780014,10.2563005695556,5.68597389417424));
#9947=CARTESIAN_POINT('Ctrl Pts',(0.204707379175836,10.2045775540887,5.68246056146672));
#9948=CARTESIAN_POINT('Ctrl Pts',(0.21,10.1764270710143,5.68148212005091));
#9949=CARTESIAN_POINT('Ctrl Pts',(0.21,10.15,5.68148212005091));
#9950=CARTESIAN_POINT('',(-0.133884278389959,10.3117868968736,5.09));
#9951=CARTESIAN_POINT('Origin',(0.,10.15,5.09));
#9952=CARTESIAN_POINT('Ctrl Pts',(0.13388427838996,10.3117868968736,5.09));
#9953=CARTESIAN_POINT('Ctrl Pts',(0.118254395260805,10.3247211682176,5.09354677224418));
#9954=CARTESIAN_POINT('Ctrl Pts',(0.1001097876823,10.3357993165874,5.09698224789957));
#9955=CARTESIAN_POINT('Ctrl Pts',(0.054829872132519,10.3546385610544,5.1030741628997));
#9956=CARTESIAN_POINT('Ctrl Pts',(0.0266020595922903,10.36,5.105));
#9957=CARTESIAN_POINT('Ctrl Pts',(-0.0266020595922903,10.36,5.105));
#9958=CARTESIAN_POINT('Ctrl Pts',(-0.0548298721325189,10.3546385610544,
5.1030741628997));
#9959=CARTESIAN_POINT('Ctrl Pts',(-0.1001097876823,10.3357993165874,5.09698224789957));
#9960=CARTESIAN_POINT('Ctrl Pts',(-0.118254395260804,10.3247211682176,5.09354677224418));
#9961=CARTESIAN_POINT('Ctrl Pts',(-0.133884278389959,10.3117868968736,5.09));
#9962=CARTESIAN_POINT('Origin',(0.,10.15,5.09));
#9963=CARTESIAN_POINT('',(-0.133884278389959,9.75,5.09));
#9964=CARTESIAN_POINT('Origin',(0.,9.75,4.5));
#9965=CARTESIAN_POINT('',(-0.605,10.55,4.5));
#9966=CARTESIAN_POINT('Origin',(0.,10.55,4.5));
#9967=CARTESIAN_POINT('',(-0.605,9.75,4.5));
#9968=CARTESIAN_POINT('',(-0.605,9.75,4.5));
#9969=CARTESIAN_POINT('Origin',(0.,9.75,4.5));
#9970=CARTESIAN_POINT('Origin',(0.,9.75,4.5));
#9971=CARTESIAN_POINT('',(-1.2,10.55,4.5));
#9972=CARTESIAN_POINT('Origin',(0.,10.55,4.5));
#9973=CARTESIAN_POINT('',(-1.2,9.75,4.5));
#9974=CARTESIAN_POINT('',(-1.2,9.75,4.5));
#9975=CARTESIAN_POINT('Origin',(0.,9.75,4.5));
#9976=CARTESIAN_POINT('Origin',(0.,10.55,4.5));
#9977=CARTESIAN_POINT('Origin',(0.,9.75,4.5));
#9978=CARTESIAN_POINT('',(0.,0.,0.));
#9979=CARTESIAN_POINT('Origin',(-0.2,-1.,-0.78));
#9980=CARTESIAN_POINT('',(-0.2,-0.9,-0.78));
#9981=CARTESIAN_POINT('',(-0.2,-0.9,-0.565685424949238));
#9982=CARTESIAN_POINT('',(-0.2,-0.9,-0.39));
#9983=CARTESIAN_POINT('',(-0.2,0.85,-0.78));
#9984=CARTESIAN_POINT('',(-0.2,-1.,-0.78));
#9985=CARTESIAN_POINT('',(-0.2,0.85,-0.565685424949238));
#9986=CARTESIAN_POINT('',(-0.2,0.85,-0.39));
#9987=CARTESIAN_POINT('',(-0.2,0.,-0.565685424949238));
#9988=CARTESIAN_POINT('Origin',(0.2,-1.,-0.78));
#9989=CARTESIAN_POINT('',(0.2,-0.9,-0.78));
#9990=CARTESIAN_POINT('',(0.1,-0.9,-0.78));
#9991=CARTESIAN_POINT('',(0.2,0.85,-0.78));
#9992=CARTESIAN_POINT('',(0.2,-1.,-0.78));
#9993=CARTESIAN_POINT('',(0.1,0.85,-0.78));
#9994=CARTESIAN_POINT('',(-0.125,-0.5,-0.78));
#9995=CARTESIAN_POINT('Origin',(0.,-0.5,-0.78));
#9996=CARTESIAN_POINT('Origin',(0.2,-1.,0.));
#9997=CARTESIAN_POINT('',(0.2,-0.9,-0.565685424949238));
#9998=CARTESIAN_POINT('',(0.2,-0.9,0.));
#9999=CARTESIAN_POINT('',(0.2,0.85,-0.565685424949238));
#10000=CARTESIAN_POINT('',(0.2,0.,-0.565685424949238));
#10001=CARTESIAN_POINT('',(0.2,0.85,0.));
#10002=CARTESIAN_POINT('Origin',(0.,0.85,0.));
#10003=CARTESIAN_POINT('',(-1.4,0.85,1.71450551880629E-16));
#10004=CARTESIAN_POINT('Origin',(0.,0.85,0.));
#10005=CARTESIAN_POINT('Origin',(0.,0.85,0.));
#10006=CARTESIAN_POINT('Origin',(0.,0.,0.));
#10007=CARTESIAN_POINT('Origin',(0.,-0.9,0.));
#10008=CARTESIAN_POINT('',(0.125,-0.5,0.586834729715275));
#10009=CARTESIAN_POINT('',(-0.125,-0.5,0.586834729715275));
#10010=CARTESIAN_POINT('Ctrl Pts',(0.125,-0.5,0.586834729715275));
#10011=CARTESIAN_POINT('Ctrl Pts',(0.125,-0.484254474936005,0.586834729715275));
#10012=CARTESIAN_POINT('Ctrl Pts',(0.121843784097853,-0.467492086231842,
0.587534197873268));
#10013=CARTESIAN_POINT('Ctrl Pts',(0.109073016834181,-0.436709004341607,
0.590038488226116));
#10014=CARTESIAN_POINT('Ctrl Pts',(0.0994608796208941,-0.422684184324257,
0.591804743154611));
#10015=CARTESIAN_POINT('Ctrl Pts',(0.077316548567853,-0.400539853271216,
0.59510289473619));
#10016=CARTESIAN_POINT('Ctrl Pts',(0.0632914182239686,-0.390927142361291,
0.596852269967858));
#10017=CARTESIAN_POINT('Ctrl Pts',(0.0325072544867634,-0.378155958502111,
0.599317707212167));
#10018=CARTESIAN_POINT('Ctrl Pts',(0.0157444828659572,-0.375,0.6));
#10019=CARTESIAN_POINT('Ctrl Pts',(-0.0157444828659573,-0.375,0.6));
#10020=CARTESIAN_POINT('Ctrl Pts',(-0.0325072544867634,-0.378155958502111,
0.599317707212167));
#10021=CARTESIAN_POINT('Ctrl Pts',(-0.0632914182239687,-0.390927142361291,
0.596852269967858));
#10022=CARTESIAN_POINT('Ctrl Pts',(-0.077316548567853,-0.400539853271216,
0.59510289473619));
#10023=CARTESIAN_POINT('Ctrl Pts',(-0.0994608796208942,-0.422684184324257,
0.591804743154611));
#10024=CARTESIAN_POINT('Ctrl Pts',(-0.109073016834181,-0.436709004341607,
0.590038488226116));
#10025=CARTESIAN_POINT('Ctrl Pts',(-0.121843784097853,-0.467492086231842,
0.587534197873268));
#10026=CARTESIAN_POINT('Ctrl Pts',(-0.125,-0.484254474936005,0.586834729715275));
#10027=CARTESIAN_POINT('Ctrl Pts',(-0.125,-0.5,0.586834729715275));
#10028=CARTESIAN_POINT('Ctrl Pts',(-0.125,-0.5,0.586834729715275));
#10029=CARTESIAN_POINT('Ctrl Pts',(-0.125,-0.515745525063995,0.586834729715275));
#10030=CARTESIAN_POINT('Ctrl Pts',(-0.121843784097853,-0.532507913768158,
0.587534197873268));
#10031=CARTESIAN_POINT('Ctrl Pts',(-0.109073016834181,-0.563290995658393,
0.590038488226116));
#10032=CARTESIAN_POINT('Ctrl Pts',(-0.0994608796208941,-0.577315815675743,
0.591804743154611));
#10033=CARTESIAN_POINT('Ctrl Pts',(-0.077316548567853,-0.599460146728784,
0.59510289473619));
#10034=CARTESIAN_POINT('Ctrl Pts',(-0.0632914182239687,-0.609072857638709,
0.596852269967858));
#10035=CARTESIAN_POINT('Ctrl Pts',(-0.0325072544867635,-0.621844041497889,
0.599317707212167));
#10036=CARTESIAN_POINT('Ctrl Pts',(-0.0157444828659572,-0.625,0.6));
#10037=CARTESIAN_POINT('Ctrl Pts',(0.0157444828659572,-0.625,0.6));
#10038=CARTESIAN_POINT('Ctrl Pts',(0.0325072544867633,-0.621844041497889,
0.599317707212167));
#10039=CARTESIAN_POINT('Ctrl Pts',(0.0632914182239686,-0.609072857638709,
0.596852269967858));
#10040=CARTESIAN_POINT('Ctrl Pts',(0.077316548567853,-0.599460146728784,
0.59510289473619));
#10041=CARTESIAN_POINT('Ctrl Pts',(0.0994608796208942,-0.577315815675743,
0.591804743154611));
#10042=CARTESIAN_POINT('Ctrl Pts',(0.109073016834181,-0.563290995658393,
0.590038488226116));
#10043=CARTESIAN_POINT('Ctrl Pts',(0.121843784097853,-0.532507913768158,
0.587534197873268));
#10044=CARTESIAN_POINT('Ctrl Pts',(0.125,-0.515745525063995,0.586834729715275));
#10045=CARTESIAN_POINT('Ctrl Pts',(0.125,-0.5,0.586834729715275));
#10046=CARTESIAN_POINT('',(-0.586834729715275,-0.5,-0.125));
#10047=CARTESIAN_POINT('',(-0.586834729715275,-0.5,0.125));
#10048=CARTESIAN_POINT('Ctrl Pts',(-0.586834729715275,-0.5,-0.125));
#10049=CARTESIAN_POINT('Ctrl Pts',(-0.586834729715275,-0.515745525063995,
-0.125));
#10050=CARTESIAN_POINT('Ctrl Pts',(-0.587534197873268,-0.532507913768158,
-0.121843784097853));
#10051=CARTESIAN_POINT('Ctrl Pts',(-0.590038488226116,-0.563290995658393,
-0.109073016834181));
#10052=CARTESIAN_POINT('Ctrl Pts',(-0.591804743154611,-0.577315815675743,
-0.0994608796208942));
#10053=CARTESIAN_POINT('Ctrl Pts',(-0.59510289473619,-0.599460146728784,
-0.0773165485678531));
#10054=CARTESIAN_POINT('Ctrl Pts',(-0.596852269967858,-0.609072857638709,
-0.0632914182239687));
#10055=CARTESIAN_POINT('Ctrl Pts',(-0.599317707212167,-0.621844041497889,
-0.0325072544867635));
#10056=CARTESIAN_POINT('Ctrl Pts',(-0.6,-0.625,-0.0157444828659573));
#10057=CARTESIAN_POINT('Ctrl Pts',(-0.6,-0.625,0.0157444828659572));
#10058=CARTESIAN_POINT('Ctrl Pts',(-0.599317707212167,-0.621844041497889,
0.0325072544867633));
#10059=CARTESIAN_POINT('Ctrl Pts',(-0.596852269967858,-0.609072857638709,
0.0632914182239686));
#10060=CARTESIAN_POINT('Ctrl Pts',(-0.59510289473619,-0.599460146728784,
0.077316548567853));
#10061=CARTESIAN_POINT('Ctrl Pts',(-0.591804743154611,-0.577315815675743,
0.0994608796208941));
#10062=CARTESIAN_POINT('Ctrl Pts',(-0.590038488226116,-0.563290995658393,
0.109073016834181));
#10063=CARTESIAN_POINT('Ctrl Pts',(-0.587534197873268,-0.532507913768158,
0.121843784097853));
#10064=CARTESIAN_POINT('Ctrl Pts',(-0.586834729715275,-0.515745525063995,
0.125));
#10065=CARTESIAN_POINT('Ctrl Pts',(-0.586834729715275,-0.5,0.125));
#10066=CARTESIAN_POINT('Ctrl Pts',(-0.586834729715275,-0.5,0.125));
#10067=CARTESIAN_POINT('Ctrl Pts',(-0.586834729715275,-0.484254474936005,
0.125));
#10068=CARTESIAN_POINT('Ctrl Pts',(-0.587534197873268,-0.467492086231842,
0.121843784097853));
#10069=CARTESIAN_POINT('Ctrl Pts',(-0.590038488226116,-0.436709004341607,
0.109073016834181));
#10070=CARTESIAN_POINT('Ctrl Pts',(-0.591804743154611,-0.422684184324257,
0.0994608796208941));
#10071=CARTESIAN_POINT('Ctrl Pts',(-0.59510289473619,-0.400539853271216,
0.077316548567853));
#10072=CARTESIAN_POINT('Ctrl Pts',(-0.596852269967858,-0.390927142361291,
0.0632914182239686));
#10073=CARTESIAN_POINT('Ctrl Pts',(-0.599317707212167,-0.378155958502111,
0.0325072544867634));
#10074=CARTESIAN_POINT('Ctrl Pts',(-0.6,-0.375,0.0157444828659572));
#10075=CARTESIAN_POINT('Ctrl Pts',(-0.6,-0.375,-0.0157444828659572));
#10076=CARTESIAN_POINT('Ctrl Pts',(-0.599317707212167,-0.378155958502111,
-0.0325072544867634));
#10077=CARTESIAN_POINT('Ctrl Pts',(-0.596852269967858,-0.390927142361291,
-0.0632914182239686));
#10078=CARTESIAN_POINT('Ctrl Pts',(-0.59510289473619,-0.400539853271216,
-0.077316548567853));
#10079=CARTESIAN_POINT('Ctrl Pts',(-0.591804743154611,-0.422684184324257,
-0.0994608796208942));
#10080=CARTESIAN_POINT('Ctrl Pts',(-0.590038488226116,-0.436709004341607,
-0.109073016834181));
#10081=CARTESIAN_POINT('Ctrl Pts',(-0.587534197873268,-0.467492086231842,
-0.121843784097853));
#10082=CARTESIAN_POINT('Ctrl Pts',(-0.586834729715275,-0.484254474936005,
-0.125));
#10083=CARTESIAN_POINT('Ctrl Pts',(-0.586834729715275,-0.5,-0.125));
#10084=CARTESIAN_POINT('',(0.586834729715275,-0.5,-0.125));
#10085=CARTESIAN_POINT('',(0.586834729715275,-0.5,0.125));
#10086=CARTESIAN_POINT('Ctrl Pts',(0.586834729715275,-0.5,-0.125));
#10087=CARTESIAN_POINT('Ctrl Pts',(0.586834729715275,-0.484254474936005,
-0.125));
#10088=CARTESIAN_POINT('Ctrl Pts',(0.587534197873268,-0.467492086231842,
-0.121843784097853));
#10089=CARTESIAN_POINT('Ctrl Pts',(0.590038488226116,-0.436709004341607,
-0.109073016834181));
#10090=CARTESIAN_POINT('Ctrl Pts',(0.591804743154611,-0.422684184324257,
-0.0994608796208941));
#10091=CARTESIAN_POINT('Ctrl Pts',(0.59510289473619,-0.400539853271216,
-0.0773165485678529));
#10092=CARTESIAN_POINT('Ctrl Pts',(0.596852269967858,-0.390927142361291,
-0.0632914182239686));
#10093=CARTESIAN_POINT('Ctrl Pts',(0.599317707212167,-0.378155958502111,
-0.0325072544867633));
#10094=CARTESIAN_POINT('Ctrl Pts',(0.6,-0.375,-0.0157444828659572));
#10095=CARTESIAN_POINT('Ctrl Pts',(0.6,-0.375,0.0157444828659573));
#10096=CARTESIAN_POINT('Ctrl Pts',(0.599317707212167,-0.378155958502111,
0.0325072544867635));
#10097=CARTESIAN_POINT('Ctrl Pts',(0.596852269967858,-0.390927142361291,
0.0632914182239687));
#10098=CARTESIAN_POINT('Ctrl Pts',(0.59510289473619,-0.400539853271216,
0.0773165485678531));
#10099=CARTESIAN_POINT('Ctrl Pts',(0.591804743154611,-0.422684184324257,
0.0994608796208942));
#10100=CARTESIAN_POINT('Ctrl Pts',(0.590038488226116,-0.436709004341607,
0.109073016834181));
#10101=CARTESIAN_POINT('Ctrl Pts',(0.587534197873268,-0.467492086231842,
0.121843784097853));
#10102=CARTESIAN_POINT('Ctrl Pts',(0.586834729715275,-0.484254474936005,
0.125));
#10103=CARTESIAN_POINT('Ctrl Pts',(0.586834729715275,-0.5,0.125));
#10104=CARTESIAN_POINT('Ctrl Pts',(0.586834729715275,-0.5,0.125));
#10105=CARTESIAN_POINT('Ctrl Pts',(0.586834729715275,-0.515745525063995,
0.125));
#10106=CARTESIAN_POINT('Ctrl Pts',(0.587534197873268,-0.532507913768158,
0.121843784097853));
#10107=CARTESIAN_POINT('Ctrl Pts',(0.590038488226116,-0.563290995658393,
0.109073016834181));
#10108=CARTESIAN_POINT('Ctrl Pts',(0.591804743154611,-0.577315815675743,
0.0994608796208942));
#10109=CARTESIAN_POINT('Ctrl Pts',(0.59510289473619,-0.599460146728784,
0.077316548567853));
#10110=CARTESIAN_POINT('Ctrl Pts',(0.596852269967858,-0.609072857638709,
0.0632914182239688));
#10111=CARTESIAN_POINT('Ctrl Pts',(0.599317707212167,-0.621844041497889,
0.0325072544867635));
#10112=CARTESIAN_POINT('Ctrl Pts',(0.6,-0.625,0.0157444828659573));
#10113=CARTESIAN_POINT('Ctrl Pts',(0.6,-0.625,-0.0157444828659572));
#10114=CARTESIAN_POINT('Ctrl Pts',(0.599317707212167,-0.621844041497889,
-0.0325072544867633));
#10115=CARTESIAN_POINT('Ctrl Pts',(0.596852269967858,-0.609072857638709,
-0.0632914182239685));
#10116=CARTESIAN_POINT('Ctrl Pts',(0.59510289473619,-0.599460146728784,
-0.077316548567853));
#10117=CARTESIAN_POINT('Ctrl Pts',(0.591804743154611,-0.577315815675743,
-0.0994608796208941));
#10118=CARTESIAN_POINT('Ctrl Pts',(0.590038488226116,-0.563290995658393,
-0.10907301683418));
#10119=CARTESIAN_POINT('Ctrl Pts',(0.587534197873268,-0.532507913768158,
-0.121843784097853));
#10120=CARTESIAN_POINT('Ctrl Pts',(0.586834729715275,-0.515745525063995,
-0.125));
#10121=CARTESIAN_POINT('Ctrl Pts',(0.586834729715275,-0.5,-0.125));
#10122=CARTESIAN_POINT('Origin',(0.,-0.5,0.));
#10123=CARTESIAN_POINT('',(-1.,-0.375,-6.12323399573677E-17));
#10124=CARTESIAN_POINT('',(-0.992156741649222,-0.5,0.125));
#10125=CARTESIAN_POINT('Ctrl Pts',(-1.,-0.375,-1.00613961606655E-16));
#10126=CARTESIAN_POINT('Ctrl Pts',(-1.,-0.375,0.0157128711428661));
#10127=CARTESIAN_POINT('Ctrl Pts',(-0.999591823858855,-0.378143583103513,
0.0324619190698278));
#10128=CARTESIAN_POINT('Ctrl Pts',(-0.998116453123232,-0.390905426591754,
0.0632545375991437));
#10129=CARTESIAN_POINT('Ctrl Pts',(-0.997070068816062,-0.400522781657727,
0.0772994769543643));
#10130=CARTESIAN_POINT('Ctrl Pts',(-0.995102104277285,-0.422700615683787,
0.0994773109804239));
#10131=CARTESIAN_POINT('Ctrl Pts',(-0.994052129228928,-0.436745514765346,
0.109094593469654));
#10132=CARTESIAN_POINT('Ctrl Pts',(-0.99256853061881,-0.467537996927464,
0.121856383722779));
#10133=CARTESIAN_POINT('Ctrl Pts',(-0.992156741649222,-0.484286997589363,
0.125));
#10134=CARTESIAN_POINT('Ctrl Pts',(-0.992156741649222,-0.5,0.125));
#10135=CARTESIAN_POINT('',(-1.,-0.625,-6.12323399573677E-17));
#10136=CARTESIAN_POINT('Ctrl Pts',(-1.,-0.625,-4.5102810375397E-17));
#10137=CARTESIAN_POINT('Ctrl Pts',(-1.,-0.625,-0.0157128711428662));
#10138=CARTESIAN_POINT('Ctrl Pts',(-0.999591823858855,-0.621856416896487,
-0.032461919069828));
#10139=CARTESIAN_POINT('Ctrl Pts',(-0.998116453123232,-0.609094573408246,
-0.0632545375991439));
#10140=CARTESIAN_POINT('Ctrl Pts',(-0.997070068816062,-0.599477218342273,
-0.0772994769543645));
#10141=CARTESIAN_POINT('Ctrl Pts',(-0.995102104277285,-0.577299384316213,
-0.0994773109804241));
#10142=CARTESIAN_POINT('Ctrl Pts',(-0.994052129228928,-0.563254485234654,
-0.109094593469655));
#10143=CARTESIAN_POINT('Ctrl Pts',(-0.99256853061881,-0.532462003072536,
-0.121856383722779));
#10144=CARTESIAN_POINT('Ctrl Pts',(-0.992156741649221,-0.515713002410637,
-0.125));
#10145=CARTESIAN_POINT('Ctrl Pts',(-0.992156741649221,-0.484286997589363,
-0.125));
#10146=CARTESIAN_POINT('Ctrl Pts',(-0.99256853061881,-0.467537996927464,
-0.121856383722779));
#10147=CARTESIAN_POINT('Ctrl Pts',(-0.994052129228928,-0.436745514765346,
-0.109094593469655));
#10148=CARTESIAN_POINT('Ctrl Pts',(-0.995102104277285,-0.422700615683787,
-0.0994773109804241));
#10149=CARTESIAN_POINT('Ctrl Pts',(-0.997070068816062,-0.400522781657728,
-0.0772994769543645));
#10150=CARTESIAN_POINT('Ctrl Pts',(-0.998116453123232,-0.390905426591754,
-0.063254537599144));
#10151=CARTESIAN_POINT('Ctrl Pts',(-0.999591823858855,-0.378143583103513,
-0.0324619190698281));
#10152=CARTESIAN_POINT('Ctrl Pts',(-1.,-0.375,-0.0157128711428663));
#10153=CARTESIAN_POINT('Ctrl Pts',(-1.,-0.375,-9.36750677027476E-17));
#10154=CARTESIAN_POINT('Ctrl Pts',(-0.992156741649222,-0.5,0.125));
#10155=CARTESIAN_POINT('Ctrl Pts',(-0.992156741649222,-0.515713002410637,
0.125));
#10156=CARTESIAN_POINT('Ctrl Pts',(-0.99256853061881,-0.532462003072536,
0.121856383722779));
#10157=CARTESIAN_POINT('Ctrl Pts',(-0.994052129228928,-0.563254485234654,
0.109094593469654));
#10158=CARTESIAN_POINT('Ctrl Pts',(-0.995102104277285,-0.577299384316213,
0.0994773109804241));
#10159=CARTESIAN_POINT('Ctrl Pts',(-0.997070068816062,-0.599477218342273,
0.0772994769543644));
#10160=CARTESIAN_POINT('Ctrl Pts',(-0.998116453123232,-0.609094573408246,
0.0632545375991438));
#10161=CARTESIAN_POINT('Ctrl Pts',(-0.999591823858855,-0.621856416896487,
0.0324619190698279));
#10162=CARTESIAN_POINT('Ctrl Pts',(-1.,-0.625,0.0157128711428661));
#10163=CARTESIAN_POINT('Ctrl Pts',(-1.,-0.625,-4.85722573273506E-17));
#10164=CARTESIAN_POINT('',(-7.65404249467096E-18,-0.5,0.125));
#10165=CARTESIAN_POINT('Origin',(0.,-0.5,0.));
#10166=CARTESIAN_POINT('',(0.992156741649222,-0.5,0.125));
#10167=CARTESIAN_POINT('',(-7.65404249467096E-18,-0.5,0.125));
#10168=CARTESIAN_POINT('',(1.,-0.625,6.12323399573677E-17));
#10169=CARTESIAN_POINT('Ctrl Pts',(1.,-0.625,7.28583859910259E-17));
#10170=CARTESIAN_POINT('Ctrl Pts',(1.,-0.625,0.0157128711428663));
#10171=CARTESIAN_POINT('Ctrl Pts',(0.999591823858855,-0.621856416896487,
0.032461919069828));
#10172=CARTESIAN_POINT('Ctrl Pts',(0.998116453123232,-0.609094573408246,
0.0632545375991439));
#10173=CARTESIAN_POINT('Ctrl Pts',(0.997070068816062,-0.599477218342273,
0.0772994769543645));
#10174=CARTESIAN_POINT('Ctrl Pts',(0.995102104277285,-0.577299384316213,
0.0994773109804242));
#10175=CARTESIAN_POINT('Ctrl Pts',(0.994052129228928,-0.563254485234654,
0.109094593469655));
#10176=CARTESIAN_POINT('Ctrl Pts',(0.99256853061881,-0.532462003072536,
0.121856383722779));
#10177=CARTESIAN_POINT('Ctrl Pts',(0.992156741649222,-0.515713002410637,
0.125));
#10178=CARTESIAN_POINT('Ctrl Pts',(0.992156741649222,-0.5,0.125));
#10179=CARTESIAN_POINT('',(1.,-0.375,6.12323399573677E-17));
#10180=CARTESIAN_POINT('Ctrl Pts',(1.,-0.375,2.08166817117217E-17));
#10181=CARTESIAN_POINT('Ctrl Pts',(1.,-0.375,-0.0157128711428662));
#10182=CARTESIAN_POINT('Ctrl Pts',(0.999591823858855,-0.378143583103513,
-0.032461919069828));
#10183=CARTESIAN_POINT('Ctrl Pts',(0.998116453123232,-0.390905426591754,
-0.0632545375991438));
#10184=CARTESIAN_POINT('Ctrl Pts',(0.997070068816062,-0.400522781657728,
-0.0772994769543644));
#10185=CARTESIAN_POINT('Ctrl Pts',(0.995102104277285,-0.422700615683787,
-0.099477310980424));
#10186=CARTESIAN_POINT('Ctrl Pts',(0.994052129228928,-0.436745514765346,
-0.109094593469654));
#10187=CARTESIAN_POINT('Ctrl Pts',(0.99256853061881,-0.467537996927464,
-0.121856383722779));
#10188=CARTESIAN_POINT('Ctrl Pts',(0.992156741649222,-0.484286997589363,
-0.125));
#10189=CARTESIAN_POINT('Ctrl Pts',(0.992156741649222,-0.515713002410637,
-0.125));
#10190=CARTESIAN_POINT('Ctrl Pts',(0.99256853061881,-0.532462003072536,
-0.121856383722779));
#10191=CARTESIAN_POINT('Ctrl Pts',(0.994052129228928,-0.563254485234654,
-0.109094593469654));
#10192=CARTESIAN_POINT('Ctrl Pts',(0.995102104277285,-0.577299384316213,
-0.099477310980424));
#10193=CARTESIAN_POINT('Ctrl Pts',(0.997070068816062,-0.599477218342273,
-0.0772994769543643));
#10194=CARTESIAN_POINT('Ctrl Pts',(0.998116453123232,-0.609094573408246,
-0.0632545375991438));
#10195=CARTESIAN_POINT('Ctrl Pts',(0.999591823858855,-0.621856416896487,
-0.0324619190698279));
#10196=CARTESIAN_POINT('Ctrl Pts',(1.,-0.625,-0.0157128711428661));
#10197=CARTESIAN_POINT('Ctrl Pts',(1.,-0.625,8.32667268468867E-17));
#10198=CARTESIAN_POINT('Ctrl Pts',(0.992156741649222,-0.5,0.125));
#10199=CARTESIAN_POINT('Ctrl Pts',(0.992156741649222,-0.484286997589363,
0.125));
#10200=CARTESIAN_POINT('Ctrl Pts',(0.99256853061881,-0.467537996927464,
0.121856383722779));
#10201=CARTESIAN_POINT('Ctrl Pts',(0.994052129228928,-0.436745514765346,
0.109094593469654));
#10202=CARTESIAN_POINT('Ctrl Pts',(0.995102104277285,-0.422700615683787,
0.0994773109804241));
#10203=CARTESIAN_POINT('Ctrl Pts',(0.997070068816062,-0.400522781657727,
0.0772994769543644));
#10204=CARTESIAN_POINT('Ctrl Pts',(0.998116453123232,-0.390905426591754,
0.0632545375991438));
#10205=CARTESIAN_POINT('Ctrl Pts',(0.999591823858855,-0.378143583103513,
0.0324619190698279));
#10206=CARTESIAN_POINT('Ctrl Pts',(1.,-0.375,0.0157128711428662));
#10207=CARTESIAN_POINT('Ctrl Pts',(1.,-0.375,2.77555756156289E-17));
#10208=CARTESIAN_POINT('Origin',(0.,-0.1,0.));
#10209=CARTESIAN_POINT('',(-1.,-0.9,1.22464679914735E-16));
#10210=CARTESIAN_POINT('Origin',(0.,-0.9,0.));
#10211=CARTESIAN_POINT('',(-1.,-0.1,-1.22464679914735E-16));
#10212=CARTESIAN_POINT('',(-1.,-0.1,1.22464679914735E-16));
#10213=CARTESIAN_POINT('',(-1.,-0.1,-1.22464679914735E-16));
#10214=CARTESIAN_POINT('Origin',(0.,-0.1,0.));
#10215=CARTESIAN_POINT('',(0.,-0.625,-1.));
#10216=CARTESIAN_POINT('',(0.,-0.375,-1.));
#10217=CARTESIAN_POINT('Ctrl Pts',(-2.08166817117217E-17,-0.625,-1.));
#10218=CARTESIAN_POINT('Ctrl Pts',(0.0157128711428662,-0.625,-1.));
#10219=CARTESIAN_POINT('Ctrl Pts',(0.0324619190698279,-0.621856416896487,
-0.999591823858855));
#10220=CARTESIAN_POINT('Ctrl Pts',(0.0632545375991438,-0.609094573408246,
-0.998116453123232));
#10221=CARTESIAN_POINT('Ctrl Pts',(0.0772994769543644,-0.599477218342273,
-0.997070068816062));
#10222=CARTESIAN_POINT('Ctrl Pts',(0.0994773109804241,-0.577299384316213,
-0.995102104277285));
#10223=CARTESIAN_POINT('Ctrl Pts',(0.109094593469654,-0.563254485234654,
-0.994052129228928));
#10224=CARTESIAN_POINT('Ctrl Pts',(0.121856383722779,-0.532462003072536,
-0.99256853061881));
#10225=CARTESIAN_POINT('Ctrl Pts',(0.125,-0.515713002410637,-0.992156741649221));
#10226=CARTESIAN_POINT('Ctrl Pts',(0.125,-0.484286997589363,-0.992156741649221));
#10227=CARTESIAN_POINT('Ctrl Pts',(0.121856383722779,-0.467537996927464,
-0.99256853061881));
#10228=CARTESIAN_POINT('Ctrl Pts',(0.109094593469654,-0.436745514765346,
-0.994052129228928));
#10229=CARTESIAN_POINT('Ctrl Pts',(0.0994773109804241,-0.422700615683787,
-0.995102104277285));
#10230=CARTESIAN_POINT('Ctrl Pts',(0.0772994769543645,-0.400522781657728,
-0.997070068816062));
#10231=CARTESIAN_POINT('Ctrl Pts',(0.0632545375991439,-0.390905426591754,
-0.998116453123232));
#10232=CARTESIAN_POINT('Ctrl Pts',(0.032461919069828,-0.378143583103513,
-0.999591823858855));
#10233=CARTESIAN_POINT('Ctrl Pts',(0.0157128711428662,-0.375,-1.));
#10234=CARTESIAN_POINT('Ctrl Pts',(3.81639164714898E-17,-0.375,-1.));
#10235=CARTESIAN_POINT('',(-0.125,-0.5,-0.992156741649222));
#10236=CARTESIAN_POINT('Ctrl Pts',(4.5102810375397E-17,-0.375,-1.));
#10237=CARTESIAN_POINT('Ctrl Pts',(-0.0157128711428661,-0.375,-1.));
#10238=CARTESIAN_POINT('Ctrl Pts',(-0.0324619190698279,-0.378143583103513,
-0.999591823858855));
#10239=CARTESIAN_POINT('Ctrl Pts',(-0.0632545375991437,-0.390905426591754,
-0.998116453123232));
#10240=CARTESIAN_POINT('Ctrl Pts',(-0.0772994769543643,-0.400522781657727,
-0.997070068816062));
#10241=CARTESIAN_POINT('Ctrl Pts',(-0.099477310980424,-0.422700615683787,
-0.995102104277285));
#10242=CARTESIAN_POINT('Ctrl Pts',(-0.109094593469654,-0.436745514765346,
-0.994052129228928));
#10243=CARTESIAN_POINT('Ctrl Pts',(-0.121856383722779,-0.467537996927464,
-0.99256853061881));
#10244=CARTESIAN_POINT('Ctrl Pts',(-0.125,-0.484286997589363,-0.992156741649222));
#10245=CARTESIAN_POINT('Ctrl Pts',(-0.125,-0.5,-0.992156741649222));
#10246=CARTESIAN_POINT('Ctrl Pts',(-0.125,-0.5,-0.992156741649222));
#10247=CARTESIAN_POINT('Ctrl Pts',(-0.125,-0.515713002410637,-0.992156741649222));
#10248=CARTESIAN_POINT('Ctrl Pts',(-0.121856383722779,-0.532462003072536,
-0.99256853061881));
#10249=CARTESIAN_POINT('Ctrl Pts',(-0.109094593469654,-0.563254485234654,
-0.994052129228928));
#10250=CARTESIAN_POINT('Ctrl Pts',(-0.0994773109804241,-0.577299384316213,
-0.995102104277285));
#10251=CARTESIAN_POINT('Ctrl Pts',(-0.0772994769543644,-0.599477218342273,
-0.997070068816062));
#10252=CARTESIAN_POINT('Ctrl Pts',(-0.0632545375991439,-0.609094573408246,
-0.998116453123232));
#10253=CARTESIAN_POINT('Ctrl Pts',(-0.032461919069828,-0.621856416896487,
-0.999591823858855));
#10254=CARTESIAN_POINT('Ctrl Pts',(-0.0157128711428662,-0.625,-1.));
#10255=CARTESIAN_POINT('Ctrl Pts',(-1.38777878078145E-17,-0.625,-1.));
#10256=CARTESIAN_POINT('',(0.,-0.375,1.));
#10257=CARTESIAN_POINT('',(0.,-0.625,1.));
#10258=CARTESIAN_POINT('Ctrl Pts',(4.16333634234434E-17,-0.375,1.));
#10259=CARTESIAN_POINT('Ctrl Pts',(0.0157128711428662,-0.375,1.));
#10260=CARTESIAN_POINT('Ctrl Pts',(0.032461919069828,-0.378143583103513,
0.999591823858855));
#10261=CARTESIAN_POINT('Ctrl Pts',(0.0632545375991439,-0.390905426591754,
0.998116453123232));
#10262=CARTESIAN_POINT('Ctrl Pts',(0.0772994769543644,-0.400522781657728,
0.997070068816062));
#10263=CARTESIAN_POINT('Ctrl Pts',(0.0994773109804241,-0.422700615683787,
0.995102104277285));
#10264=CARTESIAN_POINT('Ctrl Pts',(0.109094593469654,-0.436745514765346,
0.994052129228928));
#10265=CARTESIAN_POINT('Ctrl Pts',(0.121856383722779,-0.467537996927464,
0.99256853061881));
#10266=CARTESIAN_POINT('Ctrl Pts',(0.125,-0.484286997589363,0.992156741649222));
#10267=CARTESIAN_POINT('Ctrl Pts',(0.125,-0.515713002410637,0.992156741649222));
#10268=CARTESIAN_POINT('Ctrl Pts',(0.121856383722779,-0.532462003072536,
0.99256853061881));
#10269=CARTESIAN_POINT('Ctrl Pts',(0.109094593469655,-0.563254485234654,
0.994052129228928));
#10270=CARTESIAN_POINT('Ctrl Pts',(0.0994773109804241,-0.577299384316213,
0.995102104277285));
#10271=CARTESIAN_POINT('Ctrl Pts',(0.0772994769543644,-0.599477218342273,
0.997070068816062));
#10272=CARTESIAN_POINT('Ctrl Pts',(0.0632545375991438,-0.609094573408246,
0.998116453123232));
#10273=CARTESIAN_POINT('Ctrl Pts',(0.0324619190698279,-0.621856416896487,
0.999591823858855));
#10274=CARTESIAN_POINT('Ctrl Pts',(0.0157128711428662,-0.625,1.));
#10275=CARTESIAN_POINT('Ctrl Pts',(-1.73472347597681E-17,-0.625,1.));
#10276=CARTESIAN_POINT('',(-0.125,-0.5,0.992156741649222));
#10277=CARTESIAN_POINT('Ctrl Pts',(-1.73472347597681E-17,-0.625,1.));
#10278=CARTESIAN_POINT('Ctrl Pts',(-0.0157128711428662,-0.625,1.));
#10279=CARTESIAN_POINT('Ctrl Pts',(-0.032461919069828,-0.621856416896487,
0.999591823858855));
#10280=CARTESIAN_POINT('Ctrl Pts',(-0.0632545375991439,-0.609094573408246,
0.998116453123232));
#10281=CARTESIAN_POINT('Ctrl Pts',(-0.0772994769543645,-0.599477218342273,
0.997070068816062));
#10282=CARTESIAN_POINT('Ctrl Pts',(-0.0994773109804241,-0.577299384316213,
0.995102104277285));
#10283=CARTESIAN_POINT('Ctrl Pts',(-0.109094593469654,-0.563254485234654,
0.994052129228928));
#10284=CARTESIAN_POINT('Ctrl Pts',(-0.121856383722779,-0.532462003072536,
0.99256853061881));
#10285=CARTESIAN_POINT('Ctrl Pts',(-0.125,-0.515713002410637,0.992156741649222));
#10286=CARTESIAN_POINT('Ctrl Pts',(-0.125,-0.5,0.992156741649222));
#10287=CARTESIAN_POINT('Ctrl Pts',(-0.125,-0.5,0.992156741649222));
#10288=CARTESIAN_POINT('Ctrl Pts',(-0.125,-0.484286997589363,0.992156741649222));
#10289=CARTESIAN_POINT('Ctrl Pts',(-0.121856383722779,-0.467537996927464,
0.99256853061881));
#10290=CARTESIAN_POINT('Ctrl Pts',(-0.109094593469654,-0.436745514765346,
0.994052129228928));
#10291=CARTESIAN_POINT('Ctrl Pts',(-0.099477310980424,-0.422700615683787,
0.995102104277285));
#10292=CARTESIAN_POINT('Ctrl Pts',(-0.0772994769543643,-0.400522781657727,
0.997070068816062));
#10293=CARTESIAN_POINT('Ctrl Pts',(-0.0632545375991438,-0.390905426591754,
0.998116453123232));
#10294=CARTESIAN_POINT('Ctrl Pts',(-0.0324619190698279,-0.378143583103513,
0.999591823858855));
#10295=CARTESIAN_POINT('Ctrl Pts',(-0.0157128711428661,-0.375,1.));
#10296=CARTESIAN_POINT('Ctrl Pts',(4.5102810375397E-17,-0.375,1.));
#10297=CARTESIAN_POINT('Origin',(0.,-0.5,0.));
#10298=CARTESIAN_POINT('',(-0.125,-0.5,0.));
#10299=CARTESIAN_POINT('Origin',(0.,-0.5,0.));
#10300=CARTESIAN_POINT('',(-0.125,-0.5,0.));
#10301=CARTESIAN_POINT('Origin',(0.,-0.9,0.));
#10302=CARTESIAN_POINT('Origin',(0.,0.,0.));
#10303=CARTESIAN_POINT('',(-1.4,0.,1.71450551880629E-16));
#10304=CARTESIAN_POINT('Origin',(0.,0.,0.));
#10305=CARTESIAN_POINT('',(1.23958209161204,0.,0.143317017690053));
#10306=CARTESIAN_POINT('',(1.22320001975977,0.,0.246749348660852));
#10307=CARTESIAN_POINT('Origin',(1.21321664662686,0.,0.192154639568406));
#10308=CARTESIAN_POINT('',(1.20190105810224,0.,0.335465908756113));
#10309=CARTESIAN_POINT('Origin',(0.,0.,0.));
#10310=CARTESIAN_POINT('',(1.16954029537568,0.,0.435062095450087));
#10311=CARTESIAN_POINT('Origin',(1.1682203282434,0.,0.379577794185952));
#10312=CARTESIAN_POINT('',(1.13462523166105,0.,0.519354515801077));
#10313=CARTESIAN_POINT('Origin',(0.,0.,0.));
#10314=CARTESIAN_POINT('',(1.08708260743774,0.,0.612662169561029));
#10315=CARTESIAN_POINT('Origin',(1.0944585482776,0.,0.557654483764164));
#10316=CARTESIAN_POINT('',(1.0394111664111,0.,0.690454891028201));
#10317=CARTESIAN_POINT('Origin',(0.,0.,0.));
#10318=CARTESIAN_POINT('',(0.977857337884349,0.,0.775176467748211));
#10319=CARTESIAN_POINT('Origin',(0.993747566553533,0.,0.72199986920298));
#10320=CARTESIAN_POINT('',(0.918603348636233,0.,0.844553975349804));
#10321=CARTESIAN_POINT('Origin',(0.,0.,0.));
#10322=CARTESIAN_POINT('',(0.844553975349804,0.,0.918603348636233));
#10323=CARTESIAN_POINT('Origin',(0.86856722168183,0.,0.86856722168183));
#10324=CARTESIAN_POINT('',(0.775176467748211,0.,0.977857337884349));
#10325=CARTESIAN_POINT('Origin',(0.,0.,0.));
#10326=CARTESIAN_POINT('',(0.690454891028201,0.,1.0394111664111));
#10327=CARTESIAN_POINT('Origin',(0.721999869202979,0.,0.993747566553533));
#10328=CARTESIAN_POINT('',(0.612662169561028,0.,1.08708260743774));
#10329=CARTESIAN_POINT('Origin',(0.,0.,0.));
#10330=CARTESIAN_POINT('',(0.519354515801077,0.,1.13462523166105));
#10331=CARTESIAN_POINT('Origin',(0.557654483764164,0.,1.0944585482776));
#10332=CARTESIAN_POINT('',(0.435062095450087,0.,1.16954029537568));
#10333=CARTESIAN_POINT('Origin',(0.,0.,0.));
#10334=CARTESIAN_POINT('',(0.335465908756113,0.,1.20190105810224));
#10335=CARTESIAN_POINT('Origin',(0.379577794185951,0.,1.1682203282434));
#10336=CARTESIAN_POINT('',(0.246749348660851,0.,1.22320001975977));
#10337=CARTESIAN_POINT('Origin',(0.,0.,0.));
#10338=CARTESIAN_POINT('',(0.143317017690053,0.,1.23958209161204));
#10339=CARTESIAN_POINT('Origin',(0.192154639568406,0.,1.21321664662686));
#10340=CARTESIAN_POINT('',(0.0523608139934478,0.,1.24674050008925));
#10341=CARTESIAN_POINT('Origin',(0.,0.,0.));
#10342=CARTESIAN_POINT('',(-0.0523608139934483,0.,1.24674050008925));
#10343=CARTESIAN_POINT('Origin',(-2.25642313758905E-16,0.,1.22833954473516));
#10344=CARTESIAN_POINT('',(-0.143317017690053,0.,1.23958209161204));
#10345=CARTESIAN_POINT('Origin',(0.,0.,0.));
#10346=CARTESIAN_POINT('',(-0.246749348660852,0.,1.22320001975977));
#10347=CARTESIAN_POINT('Origin',(-0.192154639568406,0.,1.21321664662686));
#10348=CARTESIAN_POINT('',(-0.335465908756113,0.,1.20190105810224));
#10349=CARTESIAN_POINT('Origin',(0.,0.,0.));
#10350=CARTESIAN_POINT('',(-0.435062095450087,0.,1.16954029537568));
#10351=CARTESIAN_POINT('Origin',(-0.379577794185951,0.,1.1682203282434));
#10352=CARTESIAN_POINT('',(-0.519354515801077,0.,1.13462523166105));
#10353=CARTESIAN_POINT('Origin',(0.,0.,0.));
#10354=CARTESIAN_POINT('',(-0.612662169561029,0.,1.08708260743774));
#10355=CARTESIAN_POINT('Origin',(-0.557654483764164,0.,1.0944585482776));
#10356=CARTESIAN_POINT('',(-0.690454891028201,0.,1.0394111664111));
#10357=CARTESIAN_POINT('Origin',(0.,0.,0.));
#10358=CARTESIAN_POINT('',(-0.775176467748211,0.,0.977857337884349));
#10359=CARTESIAN_POINT('Origin',(-0.721999869202979,0.,0.993747566553533));
#10360=CARTESIAN_POINT('',(-0.844553975349804,0.,0.918603348636233));
#10361=CARTESIAN_POINT('Origin',(0.,0.,0.));
#10362=CARTESIAN_POINT('',(-0.918603348636233,0.,0.844553975349804));
#10363=CARTESIAN_POINT('Origin',(-0.86856722168183,0.,0.86856722168183));
#10364=CARTESIAN_POINT('',(-0.977857337884348,0.,0.775176467748211));
#10365=CARTESIAN_POINT('Origin',(0.,0.,0.));
#10366=CARTESIAN_POINT('',(-1.0394111664111,0.,0.690454891028201));
#10367=CARTESIAN_POINT('Origin',(-0.993747566553533,0.,0.721999869202979));
#10368=CARTESIAN_POINT('',(-1.08708260743774,0.,0.612662169561028));
#10369=CARTESIAN_POINT('Origin',(0.,0.,0.));
#10370=CARTESIAN_POINT('',(-1.13462523166105,0.,0.519354515801077));
#10371=CARTESIAN_POINT('Origin',(-1.0944585482776,0.,0.557654483764164));
#10372=CARTESIAN_POINT('',(-1.16954029537568,0.,0.435062095450087));
#10373=CARTESIAN_POINT('Origin',(0.,0.,0.));
#10374=CARTESIAN_POINT('',(-1.20190105810224,0.,0.335465908756113));
#10375=CARTESIAN_POINT('Origin',(-1.1682203282434,0.,0.379577794185951));
#10376=CARTESIAN_POINT('',(-1.22320001975977,0.,0.246749348660851));
#10377=CARTESIAN_POINT('Origin',(0.,0.,0.));
#10378=CARTESIAN_POINT('',(-1.23958209161204,0.,0.143317017690053));
#10379=CARTESIAN_POINT('Origin',(-1.21321664662686,0.,0.192154639568406));
#10380=CARTESIAN_POINT('',(-1.24674050008925,0.,0.0523608139934479));
#10381=CARTESIAN_POINT('Origin',(0.,0.,0.));
#10382=CARTESIAN_POINT('',(-1.24674050008925,0.,-0.0523608139934482));
#10383=CARTESIAN_POINT('Origin',(-1.22833954473516,0.,-1.50428209172603E-16));
#10384=CARTESIAN_POINT('',(-1.23958209161204,0.,-0.143317017690053));
#10385=CARTESIAN_POINT('Origin',(0.,0.,0.));
#10386=CARTESIAN_POINT('',(-1.22320001975977,0.,-0.246749348660852));
#10387=CARTESIAN_POINT('Origin',(-1.21321664662686,0.,-0.192154639568406));
#10388=CARTESIAN_POINT('',(-1.20190105810224,0.,-0.335465908756113));
#10389=CARTESIAN_POINT('Origin',(0.,0.,0.));
#10390=CARTESIAN_POINT('',(-1.16954029537568,0.,-0.435062095450087));
#10391=CARTESIAN_POINT('Origin',(-1.1682203282434,0.,-0.379577794185951));
#10392=CARTESIAN_POINT('',(-1.13462523166105,0.,-0.519354515801077));
#10393=CARTESIAN_POINT('Origin',(0.,0.,0.));
#10394=CARTESIAN_POINT('',(-1.08708260743774,0.,-0.612662169561029));
#10395=CARTESIAN_POINT('Origin',(-1.0944585482776,0.,-0.557654483764164));
#10396=CARTESIAN_POINT('',(-1.0394111664111,0.,-0.690454891028201));
#10397=CARTESIAN_POINT('Origin',(0.,0.,0.));
#10398=CARTESIAN_POINT('',(-0.977857337884349,0.,-0.775176467748211));
#10399=CARTESIAN_POINT('Origin',(-0.993747566553533,0.,-0.721999869202979));
#10400=CARTESIAN_POINT('',(-0.918603348636233,0.,-0.844553975349804));
#10401=CARTESIAN_POINT('Origin',(0.,0.,0.));
#10402=CARTESIAN_POINT('',(-0.844553975349804,0.,-0.918603348636233));
#10403=CARTESIAN_POINT('Origin',(-0.86856722168183,0.,-0.86856722168183));
#10404=CARTESIAN_POINT('',(-0.775176467748211,0.,-0.977857337884348));
#10405=CARTESIAN_POINT('Origin',(0.,0.,0.));
#10406=CARTESIAN_POINT('',(-0.690454891028201,0.,-1.0394111664111));
#10407=CARTESIAN_POINT('Origin',(-0.721999869202979,0.,-0.993747566553533));
#10408=CARTESIAN_POINT('',(-0.612662169561028,0.,-1.08708260743774));
#10409=CARTESIAN_POINT('Origin',(0.,0.,0.));
#10410=CARTESIAN_POINT('',(-0.519354515801077,0.,-1.13462523166105));
#10411=CARTESIAN_POINT('Origin',(-0.557654483764164,0.,-1.0944585482776));
#10412=CARTESIAN_POINT('',(-0.435062095450087,0.,-1.16954029537568));
#10413=CARTESIAN_POINT('Origin',(0.,0.,0.));
#10414=CARTESIAN_POINT('',(-0.335465908756113,0.,-1.20190105810224));
#10415=CARTESIAN_POINT('Origin',(-0.379577794185951,0.,-1.1682203282434));
#10416=CARTESIAN_POINT('',(-0.246749348660852,0.,-1.22320001975977));
#10417=CARTESIAN_POINT('Origin',(0.,0.,0.));
#10418=CARTESIAN_POINT('',(-0.143317017690053,0.,-1.23958209161204));
#10419=CARTESIAN_POINT('Origin',(-0.192154639568406,0.,-1.21321664662686));
#10420=CARTESIAN_POINT('',(-0.0523608139934479,0.,-1.24674050008925));
#10421=CARTESIAN_POINT('Origin',(0.,0.,0.));
#10422=CARTESIAN_POINT('',(0.0523608139934481,0.,-1.24674050008925));
#10423=CARTESIAN_POINT('Origin',(7.52141045863017E-17,0.,-1.22833954473516));
#10424=CARTESIAN_POINT('',(0.143317017690053,0.,-1.23958209161204));
#10425=CARTESIAN_POINT('Origin',(0.,0.,0.));
#10426=CARTESIAN_POINT('',(0.246749348660852,0.,-1.22320001975977));
#10427=CARTESIAN_POINT('Origin',(0.192154639568406,0.,-1.21321664662686));
#10428=CARTESIAN_POINT('',(0.335465908756113,0.,-1.20190105810224));
#10429=CARTESIAN_POINT('Origin',(0.,0.,0.));
#10430=CARTESIAN_POINT('',(0.435062095450087,0.,-1.16954029537568));
#10431=CARTESIAN_POINT('Origin',(0.379577794185951,0.,-1.1682203282434));
#10432=CARTESIAN_POINT('',(0.519354515801077,0.,-1.13462523166105));
#10433=CARTESIAN_POINT('Origin',(0.,0.,0.));
#10434=CARTESIAN_POINT('',(0.612662169561028,0.,-1.08708260743774));
#10435=CARTESIAN_POINT('Origin',(0.557654483764164,0.,-1.0944585482776));
#10436=CARTESIAN_POINT('',(0.690454891028201,0.,-1.0394111664111));
#10437=CARTESIAN_POINT('Origin',(0.,0.,0.));
#10438=CARTESIAN_POINT('',(0.775176467748211,0.,-0.977857337884349));
#10439=CARTESIAN_POINT('Origin',(0.721999869202979,0.,-0.993747566553533));
#10440=CARTESIAN_POINT('',(0.844553975349804,0.,-0.918603348636233));
#10441=CARTESIAN_POINT('Origin',(0.,0.,0.));
#10442=CARTESIAN_POINT('',(0.918603348636233,0.,-0.844553975349804));
#10443=CARTESIAN_POINT('Origin',(0.86856722168183,0.,-0.86856722168183));
#10444=CARTESIAN_POINT('',(0.977857337884349,0.,-0.775176467748211));
#10445=CARTESIAN_POINT('Origin',(0.,0.,0.));
#10446=CARTESIAN_POINT('',(1.0394111664111,0.,-0.690454891028201));
#10447=CARTESIAN_POINT('Origin',(0.993747566553533,0.,-0.721999869202979));
#10448=CARTESIAN_POINT('',(1.08708260743774,0.,-0.612662169561028));
#10449=CARTESIAN_POINT('Origin',(0.,0.,0.));
#10450=CARTESIAN_POINT('',(1.13462523166105,0.,-0.519354515801077));
#10451=CARTESIAN_POINT('Origin',(1.0944585482776,0.,-0.557654483764164));
#10452=CARTESIAN_POINT('',(1.16954029537568,0.,-0.43506209545009));
#10453=CARTESIAN_POINT('Origin',(0.,0.,0.));
#10454=CARTESIAN_POINT('',(1.20190105810224,0.,-0.33546590875611));
#10455=CARTESIAN_POINT('Origin',(1.1682203282434,0.,-0.379577794185951));
#10456=CARTESIAN_POINT('',(1.22320001975977,0.,-0.246749348660852));
#10457=CARTESIAN_POINT('Origin',(0.,0.,0.));
#10458=CARTESIAN_POINT('',(1.23958209161204,0.,-0.143317017690053));
#10459=CARTESIAN_POINT('Origin',(1.21321664662686,0.,-0.192154639568406));
#10460=CARTESIAN_POINT('',(1.24674050008925,0.,-0.052360813993451));
#10461=CARTESIAN_POINT('Origin',(0.,0.,0.));
#10462=CARTESIAN_POINT('',(1.24674050008925,0.,0.052360813993451));
#10463=CARTESIAN_POINT('Origin',(1.22833954473516,0.,0.));
#10464=CARTESIAN_POINT('Origin',(0.,0.,0.));
#10465=CARTESIAN_POINT('Origin',(0.,0.,0.));
#10466=CARTESIAN_POINT('',(-1.4,-0.1,1.71450551880629E-16));
#10467=CARTESIAN_POINT('Origin',(0.,-0.1,0.));
#10468=CARTESIAN_POINT('',(-1.4,0.,-1.71450551880629E-16));
#10469=CARTESIAN_POINT('Origin',(0.,-0.1,0.));
#10470=CARTESIAN_POINT('Origin',(0.,0.75,0.));
#10471=CARTESIAN_POINT('',(-1.4,0.75,1.71450551880629E-16));
#10472=CARTESIAN_POINT('Origin',(0.,0.75,0.));
#10473=CARTESIAN_POINT('',(1.22320001975977,0.75,0.246749348660852));
#10474=CARTESIAN_POINT('',(1.23958209161204,0.75,0.143317017690053));
#10475=CARTESIAN_POINT('Origin',(1.21321664662686,0.75,0.192154639568406));
#10476=CARTESIAN_POINT('',(1.24674050008925,0.75,0.052360813993448));
#10477=CARTESIAN_POINT('Origin',(0.,0.75,0.));
#10478=CARTESIAN_POINT('',(1.24674050008925,0.75,-0.052360813993448));
#10479=CARTESIAN_POINT('Origin',(1.22833954473516,0.75,0.));
#10480=CARTESIAN_POINT('',(1.23958209161204,0.75,-0.143317017690053));
#10481=CARTESIAN_POINT('Origin',(0.,0.75,0.));
#10482=CARTESIAN_POINT('',(1.22320001975977,0.75,-0.246749348660852));
#10483=CARTESIAN_POINT('Origin',(1.21321664662686,0.75,-0.192154639568406));
#10484=CARTESIAN_POINT('',(1.20190105810224,0.75,-0.335465908756113));
#10485=CARTESIAN_POINT('Origin',(0.,0.75,0.));
#10486=CARTESIAN_POINT('',(1.16954029537568,0.75,-0.435062095450087));
#10487=CARTESIAN_POINT('Origin',(1.1682203282434,0.75,-0.379577794185951));
#10488=CARTESIAN_POINT('',(1.13462523166105,0.75,-0.519354515801077));
#10489=CARTESIAN_POINT('Origin',(0.,0.75,0.));
#10490=CARTESIAN_POINT('',(1.08708260743774,0.75,-0.612662169561028));
#10491=CARTESIAN_POINT('Origin',(1.0944585482776,0.75,-0.557654483764164));
#10492=CARTESIAN_POINT('',(1.0394111664111,0.75,-0.690454891028201));
#10493=CARTESIAN_POINT('Origin',(0.,0.75,0.));
#10494=CARTESIAN_POINT('',(0.977857337884349,0.75,-0.775176467748211));
#10495=CARTESIAN_POINT('Origin',(0.993747566553533,0.75,-0.721999869202979));
#10496=CARTESIAN_POINT('',(0.918603348636233,0.75,-0.844553975349804));
#10497=CARTESIAN_POINT('Origin',(0.,0.75,0.));
#10498=CARTESIAN_POINT('',(0.844553975349804,0.75,-0.918603348636233));
#10499=CARTESIAN_POINT('Origin',(0.86856722168183,0.75,-0.86856722168183));
#10500=CARTESIAN_POINT('',(0.775176467748211,0.75,-0.977857337884349));
#10501=CARTESIAN_POINT('Origin',(0.,0.75,0.));
#10502=CARTESIAN_POINT('',(0.690454891028201,0.75,-1.0394111664111));
#10503=CARTESIAN_POINT('Origin',(0.721999869202979,0.75,-0.993747566553533));
#10504=CARTESIAN_POINT('',(0.612662169561028,0.75,-1.08708260743774));
#10505=CARTESIAN_POINT('Origin',(0.,0.75,0.));
#10506=CARTESIAN_POINT('',(0.519354515801077,0.75,-1.13462523166105));
#10507=CARTESIAN_POINT('Origin',(0.557654483764164,0.75,-1.0944585482776));
#10508=CARTESIAN_POINT('',(0.435062095450087,0.75,-1.16954029537568));
#10509=CARTESIAN_POINT('Origin',(0.,0.75,0.));
#10510=CARTESIAN_POINT('',(0.335465908756113,0.75,-1.20190105810224));
#10511=CARTESIAN_POINT('Origin',(0.379577794185951,0.75,-1.1682203282434));
#10512=CARTESIAN_POINT('',(0.246749348660852,0.75,-1.22320001975977));
#10513=CARTESIAN_POINT('Origin',(0.,0.75,0.));
#10514=CARTESIAN_POINT('',(0.143317017690053,0.75,-1.23958209161204));
#10515=CARTESIAN_POINT('Origin',(0.192154639568406,0.75,-1.21321664662686));
#10516=CARTESIAN_POINT('',(0.0523608139934481,0.75,-1.24674050008925));
#10517=CARTESIAN_POINT('Origin',(0.,0.75,0.));
#10518=CARTESIAN_POINT('',(-0.0523608139934479,0.75,-1.24674050008925));
#10519=CARTESIAN_POINT('Origin',(7.52141045863017E-17,0.75,-1.22833954473516));
#10520=CARTESIAN_POINT('',(-0.143317017690053,0.75,-1.23958209161204));
#10521=CARTESIAN_POINT('Origin',(0.,0.75,0.));
#10522=CARTESIAN_POINT('',(-0.246749348660852,0.75,-1.22320001975977));
#10523=CARTESIAN_POINT('Origin',(-0.192154639568406,0.75,-1.21321664662686));
#10524=CARTESIAN_POINT('',(-0.335465908756113,0.75,-1.20190105810224));
#10525=CARTESIAN_POINT('Origin',(0.,0.75,0.));
#10526=CARTESIAN_POINT('',(-0.435062095450087,0.75,-1.16954029537568));
#10527=CARTESIAN_POINT('Origin',(-0.379577794185951,0.75,-1.1682203282434));
#10528=CARTESIAN_POINT('',(-0.519354515801077,0.75,-1.13462523166105));
#10529=CARTESIAN_POINT('Origin',(0.,0.75,0.));
#10530=CARTESIAN_POINT('',(-0.612662169561028,0.75,-1.08708260743774));
#10531=CARTESIAN_POINT('Origin',(-0.557654483764164,0.75,-1.0944585482776));
#10532=CARTESIAN_POINT('',(-0.690454891028201,0.75,-1.0394111664111));
#10533=CARTESIAN_POINT('Origin',(0.,0.75,0.));
#10534=CARTESIAN_POINT('',(-0.775176467748211,0.75,-0.977857337884348));
#10535=CARTESIAN_POINT('Origin',(-0.721999869202979,0.75,-0.993747566553533));
#10536=CARTESIAN_POINT('',(-0.844553975349804,0.75,-0.918603348636233));
#10537=CARTESIAN_POINT('Origin',(0.,0.75,0.));
#10538=CARTESIAN_POINT('',(-0.918603348636233,0.75,-0.844553975349804));
#10539=CARTESIAN_POINT('Origin',(-0.86856722168183,0.75,-0.86856722168183));
#10540=CARTESIAN_POINT('',(-0.977857337884349,0.75,-0.775176467748211));
#10541=CARTESIAN_POINT('Origin',(0.,0.75,0.));
#10542=CARTESIAN_POINT('',(-1.0394111664111,0.75,-0.690454891028201));
#10543=CARTESIAN_POINT('Origin',(-0.993747566553533,0.75,-0.721999869202979));
#10544=CARTESIAN_POINT('',(-1.08708260743774,0.75,-0.612662169561029));
#10545=CARTESIAN_POINT('Origin',(0.,0.75,0.));
#10546=CARTESIAN_POINT('',(-1.13462523166105,0.75,-0.519354515801077));
#10547=CARTESIAN_POINT('Origin',(-1.0944585482776,0.75,-0.557654483764164));
#10548=CARTESIAN_POINT('',(-1.16954029537568,0.75,-0.435062095450087));
#10549=CARTESIAN_POINT('Origin',(0.,0.75,0.));
#10550=CARTESIAN_POINT('',(-1.20190105810224,0.75,-0.335465908756113));
#10551=CARTESIAN_POINT('Origin',(-1.1682203282434,0.75,-0.379577794185951));
#10552=CARTESIAN_POINT('',(-1.22320001975977,0.75,-0.246749348660852));
#10553=CARTESIAN_POINT('Origin',(0.,0.75,0.));
#10554=CARTESIAN_POINT('',(-1.23958209161204,0.75,-0.143317017690053));
#10555=CARTESIAN_POINT('Origin',(-1.21321664662686,0.75,-0.192154639568406));
#10556=CARTESIAN_POINT('',(-1.24674050008925,0.75,-0.0523608139934482));
#10557=CARTESIAN_POINT('Origin',(0.,0.75,0.));
#10558=CARTESIAN_POINT('',(-1.24674050008925,0.75,0.0523608139934479));
#10559=CARTESIAN_POINT('Origin',(-1.22833954473516,0.75,-1.50428209172603E-16));
#10560=CARTESIAN_POINT('',(-1.23958209161204,0.75,0.143317017690053));
#10561=CARTESIAN_POINT('Origin',(0.,0.75,0.));
#10562=CARTESIAN_POINT('',(-1.22320001975977,0.75,0.246749348660851));
#10563=CARTESIAN_POINT('Origin',(-1.21321664662686,0.75,0.192154639568406));
#10564=CARTESIAN_POINT('',(-1.20190105810224,0.75,0.335465908756113));
#10565=CARTESIAN_POINT('Origin',(0.,0.75,0.));
#10566=CARTESIAN_POINT('',(-1.16954029537568,0.75,0.435062095450087));
#10567=CARTESIAN_POINT('Origin',(-1.1682203282434,0.75,0.379577794185951));
#10568=CARTESIAN_POINT('',(-1.13462523166105,0.75,0.519354515801077));
#10569=CARTESIAN_POINT('Origin',(0.,0.75,0.));
#10570=CARTESIAN_POINT('',(-1.08708260743774,0.75,0.612662169561028));
#10571=CARTESIAN_POINT('Origin',(-1.0944585482776,0.75,0.557654483764164));
#10572=CARTESIAN_POINT('',(-1.0394111664111,0.75,0.690454891028201));
#10573=CARTESIAN_POINT('Origin',(0.,0.75,0.));
#10574=CARTESIAN_POINT('',(-0.977857337884348,0.75,0.775176467748211));
#10575=CARTESIAN_POINT('Origin',(-0.993747566553533,0.75,0.721999869202979));
#10576=CARTESIAN_POINT('',(-0.918603348636233,0.75,0.844553975349804));
#10577=CARTESIAN_POINT('Origin',(0.,0.75,0.));
#10578=CARTESIAN_POINT('',(-0.844553975349804,0.75,0.918603348636233));
#10579=CARTESIAN_POINT('Origin',(-0.86856722168183,0.75,0.86856722168183));
#10580=CARTESIAN_POINT('',(-0.775176467748211,0.75,0.977857337884349));
#10581=CARTESIAN_POINT('Origin',(0.,0.75,0.));
#10582=CARTESIAN_POINT('',(-0.690454891028201,0.75,1.0394111664111));
#10583=CARTESIAN_POINT('Origin',(-0.721999869202979,0.75,0.993747566553533));
#10584=CARTESIAN_POINT('',(-0.612662169561029,0.75,1.08708260743774));
#10585=CARTESIAN_POINT('Origin',(0.,0.75,0.));
#10586=CARTESIAN_POINT('',(-0.519354515801077,0.75,1.13462523166105));
#10587=CARTESIAN_POINT('Origin',(-0.557654483764164,0.75,1.0944585482776));
#10588=CARTESIAN_POINT('',(-0.435062095450087,0.75,1.16954029537568));
#10589=CARTESIAN_POINT('Origin',(0.,0.75,0.));
#10590=CARTESIAN_POINT('',(-0.335465908756113,0.75,1.20190105810224));
#10591=CARTESIAN_POINT('Origin',(-0.379577794185951,0.75,1.1682203282434));
#10592=CARTESIAN_POINT('',(-0.246749348660852,0.75,1.22320001975977));
#10593=CARTESIAN_POINT('Origin',(0.,0.75,0.));
#10594=CARTESIAN_POINT('',(-0.143317017690053,0.75,1.23958209161204));
#10595=CARTESIAN_POINT('Origin',(-0.192154639568406,0.75,1.21321664662686));
#10596=CARTESIAN_POINT('',(-0.0523608139934483,0.75,1.24674050008925));
#10597=CARTESIAN_POINT('Origin',(0.,0.75,0.));
#10598=CARTESIAN_POINT('',(0.0523608139934478,0.75,1.24674050008925));
#10599=CARTESIAN_POINT('Origin',(-2.25642313758905E-16,0.75,1.22833954473516));
#10600=CARTESIAN_POINT('',(0.143317017690053,0.75,1.23958209161204));
#10601=CARTESIAN_POINT('Origin',(0.,0.75,0.));
#10602=CARTESIAN_POINT('',(0.246749348660851,0.75,1.22320001975977));
#10603=CARTESIAN_POINT('Origin',(0.192154639568406,0.75,1.21321664662686));
#10604=CARTESIAN_POINT('',(0.335465908756113,0.75,1.20190105810224));
#10605=CARTESIAN_POINT('Origin',(0.,0.75,0.));
#10606=CARTESIAN_POINT('',(0.435062095450087,0.75,1.16954029537568));
#10607=CARTESIAN_POINT('Origin',(0.379577794185951,0.75,1.1682203282434));
#10608=CARTESIAN_POINT('',(0.519354515801077,0.75,1.13462523166105));
#10609=CARTESIAN_POINT('Origin',(0.,0.75,0.));
#10610=CARTESIAN_POINT('',(0.612662169561028,0.75,1.08708260743774));
#10611=CARTESIAN_POINT('Origin',(0.557654483764164,0.75,1.0944585482776));
#10612=CARTESIAN_POINT('',(0.690454891028201,0.75,1.0394111664111));
#10613=CARTESIAN_POINT('Origin',(0.,0.75,0.));
#10614=CARTESIAN_POINT('',(0.775176467748211,0.75,0.977857337884349));
#10615=CARTESIAN_POINT('Origin',(0.721999869202979,0.75,0.993747566553533));
#10616=CARTESIAN_POINT('',(0.844553975349804,0.75,0.918603348636233));
#10617=CARTESIAN_POINT('Origin',(0.,0.75,0.));
#10618=CARTESIAN_POINT('',(0.918603348636233,0.75,0.844553975349804));
#10619=CARTESIAN_POINT('Origin',(0.86856722168183,0.75,0.86856722168183));
#10620=CARTESIAN_POINT('',(0.977857337884349,0.75,0.775176467748211));
#10621=CARTESIAN_POINT('Origin',(0.,0.75,0.));
#10622=CARTESIAN_POINT('',(1.0394111664111,0.75,0.690454891028201));
#10623=CARTESIAN_POINT('Origin',(0.993747566553533,0.75,0.72199986920298));
#10624=CARTESIAN_POINT('',(1.08708260743774,0.75,0.612662169561029));
#10625=CARTESIAN_POINT('Origin',(0.,0.75,0.));
#10626=CARTESIAN_POINT('',(1.13462523166105,0.75,0.519354515801077));
#10627=CARTESIAN_POINT('Origin',(1.0944585482776,0.75,0.557654483764164));
#10628=CARTESIAN_POINT('',(1.16954029537568,0.75,0.435062095450087));
#10629=CARTESIAN_POINT('Origin',(0.,0.75,0.));
#10630=CARTESIAN_POINT('',(1.20190105810224,0.75,0.335465908756113));
#10631=CARTESIAN_POINT('Origin',(1.1682203282434,0.75,0.379577794185952));
#10632=CARTESIAN_POINT('Origin',(0.,0.75,0.));
#10633=CARTESIAN_POINT('Origin',(0.,0.75,0.));
#10634=CARTESIAN_POINT('',(-1.4,0.75,1.71450551880629E-16));
#10635=CARTESIAN_POINT('Origin',(1.21321664662686,0.,0.192154639568406));
#10636=CARTESIAN_POINT('',(1.23958209161204,0.,0.14331701769005));
#10637=CARTESIAN_POINT('',(1.22320001975977,0.,0.246749348660855));
#10638=CARTESIAN_POINT('Origin',(0.,0.,0.));
#10639=CARTESIAN_POINT('',(1.20190105810224,0.,0.33546590875611));
#10640=CARTESIAN_POINT('Origin',(1.1682203282434,0.,0.379577794185952));
#10641=CARTESIAN_POINT('',(1.16954029537568,0.,0.43506209545009));
#10642=CARTESIAN_POINT('Origin',(0.,0.,0.));
#10643=CARTESIAN_POINT('',(1.13462523166105,0.,0.519354515801074));
#10644=CARTESIAN_POINT('Origin',(1.0944585482776,0.,0.557654483764164));
#10645=CARTESIAN_POINT('',(1.08708260743774,0.,0.612662169561031));
#10646=CARTESIAN_POINT('Origin',(0.,0.,0.));
#10647=CARTESIAN_POINT('',(1.03941116641111,0.,0.690454891028199));
#10648=CARTESIAN_POINT('Origin',(0.993747566553533,0.,0.72199986920298));
#10649=CARTESIAN_POINT('',(0.977857337884347,0.,0.775176467748214));
#10650=CARTESIAN_POINT('Origin',(0.,0.,0.));
#10651=CARTESIAN_POINT('',(0.918603348636235,0.,0.844553975349802));
#10652=CARTESIAN_POINT('Origin',(0.86856722168183,0.,0.86856722168183));
#10653=CARTESIAN_POINT('',(0.844553975349802,0.,0.918603348636235));
#10654=CARTESIAN_POINT('Origin',(0.,0.,0.));
#10655=CARTESIAN_POINT('',(0.775176467748213,0.,0.977857337884347));
#10656=CARTESIAN_POINT('Origin',(0.721999869202979,0.,0.993747566553533));
#10657=CARTESIAN_POINT('',(0.690454891028198,0.,1.03941116641111));
#10658=CARTESIAN_POINT('Origin',(0.,0.,0.));
#10659=CARTESIAN_POINT('',(0.612662169561031,0.,1.08708260743774));
#10660=CARTESIAN_POINT('Origin',(0.557654483764164,0.,1.0944585482776));
#10661=CARTESIAN_POINT('',(0.519354515801074,0.,1.13462523166105));
#10662=CARTESIAN_POINT('Origin',(0.,0.,0.));
#10663=CARTESIAN_POINT('',(0.43506209545009,0.,1.16954029537568));
#10664=CARTESIAN_POINT('Origin',(0.379577794185951,0.,1.1682203282434));
#10665=CARTESIAN_POINT('',(0.33546590875611,0.,1.20190105810224));
#10666=CARTESIAN_POINT('Origin',(0.,0.,0.));
#10667=CARTESIAN_POINT('',(0.246749348660854,0.,1.22320001975977));
#10668=CARTESIAN_POINT('Origin',(0.192154639568406,0.,1.21321664662686));
#10669=CARTESIAN_POINT('',(0.14331701769005,0.,1.23958209161204));
#10670=CARTESIAN_POINT('Origin',(0.,0.,0.));
#10671=CARTESIAN_POINT('',(0.0523608139934508,0.,1.24674050008925));
#10672=CARTESIAN_POINT('Origin',(-2.25642313758905E-16,0.,1.22833954473516));
#10673=CARTESIAN_POINT('',(-0.0523608139934513,0.,1.24674050008925));
#10674=CARTESIAN_POINT('Origin',(0.,0.,0.));
#10675=CARTESIAN_POINT('',(-0.14331701769005,0.,1.23958209161204));
#10676=CARTESIAN_POINT('Origin',(-0.192154639568406,0.,1.21321664662686));
#10677=CARTESIAN_POINT('',(-0.246749348660855,0.,1.22320001975977));
#10678=CARTESIAN_POINT('Origin',(0.,0.,0.));
#10679=CARTESIAN_POINT('',(-0.33546590875611,0.,1.20190105810224));
#10680=CARTESIAN_POINT('Origin',(-0.379577794185951,0.,1.1682203282434));
#10681=CARTESIAN_POINT('',(-0.43506209545009,0.,1.16954029537568));
#10682=CARTESIAN_POINT('Origin',(0.,0.,0.));
#10683=CARTESIAN_POINT('',(-0.519354515801074,0.,1.13462523166105));
#10684=CARTESIAN_POINT('Origin',(-0.557654483764164,0.,1.0944585482776));
#10685=CARTESIAN_POINT('',(-0.612662169561031,0.,1.08708260743774));
#10686=CARTESIAN_POINT('Origin',(0.,0.,0.));
#10687=CARTESIAN_POINT('',(-0.690454891028199,0.,1.03941116641111));
#10688=CARTESIAN_POINT('Origin',(-0.721999869202979,0.,0.993747566553533));
#10689=CARTESIAN_POINT('',(-0.775176467748213,0.,0.977857337884347));
#10690=CARTESIAN_POINT('Origin',(0.,0.,0.));
#10691=CARTESIAN_POINT('',(-0.844553975349802,0.,0.918603348636235));
#10692=CARTESIAN_POINT('Origin',(-0.86856722168183,0.,0.86856722168183));
#10693=CARTESIAN_POINT('',(-0.918603348636235,0.,0.844553975349802));
#10694=CARTESIAN_POINT('Origin',(0.,0.,0.));
#10695=CARTESIAN_POINT('',(-0.977857337884347,0.,0.775176467748213));
#10696=CARTESIAN_POINT('Origin',(-0.993747566553533,0.,0.721999869202979));
#10697=CARTESIAN_POINT('',(-1.03941116641111,0.,0.690454891028198));
#10698=CARTESIAN_POINT('Origin',(0.,0.,0.));
#10699=CARTESIAN_POINT('',(-1.08708260743774,0.,0.612662169561031));
#10700=CARTESIAN_POINT('Origin',(-1.0944585482776,0.,0.557654483764164));
#10701=CARTESIAN_POINT('',(-1.13462523166105,0.,0.519354515801074));
#10702=CARTESIAN_POINT('Origin',(0.,0.,0.));
#10703=CARTESIAN_POINT('',(-1.16954029537568,0.,0.43506209545009));
#10704=CARTESIAN_POINT('Origin',(-1.1682203282434,0.,0.379577794185951));
#10705=CARTESIAN_POINT('',(-1.20190105810224,0.,0.33546590875611));
#10706=CARTESIAN_POINT('Origin',(0.,0.,0.));
#10707=CARTESIAN_POINT('',(-1.22320001975977,0.,0.246749348660854));
#10708=CARTESIAN_POINT('Origin',(-1.21321664662686,0.,0.192154639568406));
#10709=CARTESIAN_POINT('',(-1.23958209161204,0.,0.14331701769005));
#10710=CARTESIAN_POINT('Origin',(0.,0.,0.));
#10711=CARTESIAN_POINT('',(-1.24674050008925,0.,0.0523608139934509));
#10712=CARTESIAN_POINT('Origin',(-1.22833954473516,0.,-1.50428209172603E-16));
#10713=CARTESIAN_POINT('',(-1.24674050008925,0.,-0.0523608139934512));
#10714=CARTESIAN_POINT('Origin',(0.,0.,0.));
#10715=CARTESIAN_POINT('',(-1.23958209161204,0.,-0.14331701769005));
#10716=CARTESIAN_POINT('Origin',(-1.21321664662686,0.,-0.192154639568406));
#10717=CARTESIAN_POINT('',(-1.22320001975977,0.,-0.246749348660855));
#10718=CARTESIAN_POINT('Origin',(0.,0.,0.));
#10719=CARTESIAN_POINT('',(-1.20190105810224,0.,-0.33546590875611));
#10720=CARTESIAN_POINT('Origin',(-1.1682203282434,0.,-0.379577794185951));
#10721=CARTESIAN_POINT('',(-1.16954029537568,0.,-0.43506209545009));
#10722=CARTESIAN_POINT('Origin',(0.,0.,0.));
#10723=CARTESIAN_POINT('',(-1.13462523166105,0.,-0.519354515801074));
#10724=CARTESIAN_POINT('Origin',(-1.0944585482776,0.,-0.557654483764164));
#10725=CARTESIAN_POINT('',(-1.08708260743774,0.,-0.612662169561031));
#10726=CARTESIAN_POINT('Origin',(0.,0.,0.));
#10727=CARTESIAN_POINT('',(-1.03941116641111,0.,-0.690454891028199));
#10728=CARTESIAN_POINT('Origin',(-0.993747566553533,0.,-0.721999869202979));
#10729=CARTESIAN_POINT('',(-0.977857337884347,0.,-0.775176467748213));
#10730=CARTESIAN_POINT('Origin',(0.,0.,0.));
#10731=CARTESIAN_POINT('',(-0.918603348636235,0.,-0.844553975349802));
#10732=CARTESIAN_POINT('Origin',(-0.86856722168183,0.,-0.86856722168183));
#10733=CARTESIAN_POINT('',(-0.844553975349802,0.,-0.918603348636235));
#10734=CARTESIAN_POINT('Origin',(0.,0.,0.));
#10735=CARTESIAN_POINT('',(-0.775176467748213,0.,-0.977857337884347));
#10736=CARTESIAN_POINT('Origin',(-0.721999869202979,0.,-0.993747566553533));
#10737=CARTESIAN_POINT('',(-0.690454891028198,0.,-1.03941116641111));
#10738=CARTESIAN_POINT('Origin',(0.,0.,0.));
#10739=CARTESIAN_POINT('',(-0.612662169561031,0.,-1.08708260743774));
#10740=CARTESIAN_POINT('Origin',(-0.557654483764164,0.,-1.0944585482776));
#10741=CARTESIAN_POINT('',(-0.519354515801074,0.,-1.13462523166105));
#10742=CARTESIAN_POINT('Origin',(0.,0.,0.));
#10743=CARTESIAN_POINT('',(-0.43506209545009,0.,-1.16954029537568));
#10744=CARTESIAN_POINT('Origin',(-0.379577794185951,0.,-1.1682203282434));
#10745=CARTESIAN_POINT('',(-0.33546590875611,0.,-1.20190105810224));
#10746=CARTESIAN_POINT('Origin',(0.,0.,0.));
#10747=CARTESIAN_POINT('',(-0.246749348660854,0.,-1.22320001975977));
#10748=CARTESIAN_POINT('Origin',(-0.192154639568406,0.,-1.21321664662686));
#10749=CARTESIAN_POINT('',(-0.14331701769005,0.,-1.23958209161204));
#10750=CARTESIAN_POINT('Origin',(0.,0.,0.));
#10751=CARTESIAN_POINT('',(-0.052360813993451,0.,-1.24674050008925));
#10752=CARTESIAN_POINT('Origin',(7.52141045863017E-17,0.,-1.22833954473516));
#10753=CARTESIAN_POINT('',(0.0523608139934511,0.,-1.24674050008925));
#10754=CARTESIAN_POINT('Origin',(0.,0.,0.));
#10755=CARTESIAN_POINT('',(0.14331701769005,0.,-1.23958209161204));
#10756=CARTESIAN_POINT('Origin',(0.192154639568406,0.,-1.21321664662686));
#10757=CARTESIAN_POINT('',(0.246749348660855,0.,-1.22320001975977));
#10758=CARTESIAN_POINT('Origin',(0.,0.,0.));
#10759=CARTESIAN_POINT('',(0.33546590875611,0.,-1.20190105810224));
#10760=CARTESIAN_POINT('Origin',(0.379577794185951,0.,-1.1682203282434));
#10761=CARTESIAN_POINT('',(0.43506209545009,0.,-1.16954029537568));
#10762=CARTESIAN_POINT('Origin',(0.,0.,0.));
#10763=CARTESIAN_POINT('',(0.519354515801074,0.,-1.13462523166105));
#10764=CARTESIAN_POINT('Origin',(0.557654483764164,0.,-1.0944585482776));
#10765=CARTESIAN_POINT('',(0.612662169561031,0.,-1.08708260743774));
#10766=CARTESIAN_POINT('Origin',(0.,0.,0.));
#10767=CARTESIAN_POINT('',(0.690454891028198,0.,-1.03941116641111));
#10768=CARTESIAN_POINT('Origin',(0.721999869202979,0.,-0.993747566553533));
#10769=CARTESIAN_POINT('',(0.775176467748213,0.,-0.977857337884347));
#10770=CARTESIAN_POINT('Origin',(0.,0.,0.));
#10771=CARTESIAN_POINT('',(0.844553975349802,0.,-0.918603348636235));
#10772=CARTESIAN_POINT('Origin',(0.86856722168183,0.,-0.86856722168183));
#10773=CARTESIAN_POINT('',(0.918603348636235,0.,-0.844553975349802));
#10774=CARTESIAN_POINT('Origin',(0.,0.,0.));
#10775=CARTESIAN_POINT('',(0.977857337884347,0.,-0.775176467748213));
#10776=CARTESIAN_POINT('Origin',(0.993747566553533,0.,-0.721999869202979));
#10777=CARTESIAN_POINT('',(1.03941116641111,0.,-0.690454891028198));
#10778=CARTESIAN_POINT('Origin',(0.,0.,0.));
#10779=CARTESIAN_POINT('',(1.08708260743774,0.,-0.612662169561031));
#10780=CARTESIAN_POINT('Origin',(1.0944585482776,0.,-0.557654483764164));
#10781=CARTESIAN_POINT('',(1.13462523166105,0.,-0.519354515801074));
#10782=CARTESIAN_POINT('Origin',(0.,0.,0.));
#10783=CARTESIAN_POINT('',(1.16954029537568,0.,-0.43506209545009));
#10784=CARTESIAN_POINT('Origin',(1.1682203282434,0.,-0.379577794185951));
#10785=CARTESIAN_POINT('',(1.20190105810224,0.,-0.33546590875611));
#10786=CARTESIAN_POINT('Origin',(0.,0.,0.));
#10787=CARTESIAN_POINT('',(1.22320001975977,0.,-0.246749348660855));
#10788=CARTESIAN_POINT('Origin',(1.21321664662686,0.,-0.192154639568406));
#10789=CARTESIAN_POINT('',(1.23958209161204,0.,-0.14331701769005));
#10790=CARTESIAN_POINT('Origin',(0.,0.,0.));
#10791=CARTESIAN_POINT('',(1.24674050008925,0.,0.052360813993451));
#10792=CARTESIAN_POINT('Origin',(1.22833954473516,0.,0.));
#10793=CARTESIAN_POINT('',(1.24674050008925,0.,-0.052360813993451));
#10794=CARTESIAN_POINT('Origin',(0.,0.,0.));
#10795=CARTESIAN_POINT('',(0.,0.,0.));
#10796=CARTESIAN_POINT('Origin',(0.7,0.,0.25));
#10797=CARTESIAN_POINT('',(0.7,0.16,0.4));
#10798=CARTESIAN_POINT('',(0.7,0.2,0.36));
#10799=CARTESIAN_POINT('',(0.7,0.1675,0.3925));
#10800=CARTESIAN_POINT('',(0.7,-0.16,0.4));
#10801=CARTESIAN_POINT('',(0.7,0.,0.4));
#10802=CARTESIAN_POINT('',(0.7,-0.2,0.36));
#10803=CARTESIAN_POINT('',(0.7,-0.1675,0.3925));
#10804=CARTESIAN_POINT('',(0.7,-0.2,0.04));
#10805=CARTESIAN_POINT('',(0.7,-0.2,0.125));
#10806=CARTESIAN_POINT('',(0.7,-0.16,0.));
#10807=CARTESIAN_POINT('',(0.7,-0.1925,0.0325));
#10808=CARTESIAN_POINT('',(0.7,0.16,0.));
#10809=CARTESIAN_POINT('',(0.7,0.,0.));
#10810=CARTESIAN_POINT('',(0.7,0.2,0.04));
#10811=CARTESIAN_POINT('',(0.7,0.1925,0.0325));
#10812=CARTESIAN_POINT('',(0.7,0.2,0.125));
#10813=CARTESIAN_POINT('Origin',(-0.4,-0.18,0.02));
#10814=CARTESIAN_POINT('',(-0.7,-0.2,0.04));
#10815=CARTESIAN_POINT('',(-0.4,-0.2,0.04));
#10816=CARTESIAN_POINT('',(-0.7,-0.16,0.));
#10817=CARTESIAN_POINT('',(-0.7,-0.1925,0.0325));
#10818=CARTESIAN_POINT('',(-0.4,-0.16,0.));
#10819=CARTESIAN_POINT('Origin',(-0.8,-0.2,0.));
#10820=CARTESIAN_POINT('',(-0.7,-0.2,0.36));
#10821=CARTESIAN_POINT('',(-0.4,-0.2,0.36));
#10822=CARTESIAN_POINT('',(-0.7,-0.2,0.125));
#10823=CARTESIAN_POINT('Origin',(-0.4,-0.18,0.38));
#10824=CARTESIAN_POINT('',(-0.7,-0.16,0.4));
#10825=CARTESIAN_POINT('',(-0.4,-0.16,0.4));
#10826=CARTESIAN_POINT('',(-0.7,-0.1675,0.3925));
#10827=CARTESIAN_POINT('Origin',(0.,0.,0.4));
#10828=CARTESIAN_POINT('',(-0.7,0.16,0.4));
#10829=CARTESIAN_POINT('',(0.4,0.16,0.4));
#10830=CARTESIAN_POINT('',(-0.7,0.,0.4));
#10831=CARTESIAN_POINT('Origin',(-0.7,0.,0.25));
#10832=CARTESIAN_POINT('',(-0.7,0.2,0.36));
#10833=CARTESIAN_POINT('',(-0.7,0.1675,0.3925));
#10834=CARTESIAN_POINT('',(-0.7,0.2,0.04));
#10835=CARTESIAN_POINT('',(-0.7,0.2,0.125));
#10836=CARTESIAN_POINT('',(-0.7,0.16,0.));
#10837=CARTESIAN_POINT('',(-0.7,0.1925,0.0325));
#10838=CARTESIAN_POINT('',(-0.7,0.,0.));
#10839=CARTESIAN_POINT('Origin',(0.4,0.18,0.38));
#10840=CARTESIAN_POINT('',(0.4,0.2,0.36));
#10841=CARTESIAN_POINT('Origin',(0.8,0.2,0.));
#10842=CARTESIAN_POINT('',(0.4,0.2,0.04));
#10843=CARTESIAN_POINT('Origin',(0.4,0.18,0.02));
#10844=CARTESIAN_POINT('',(0.4,0.16,0.));
#10845=CARTESIAN_POINT('Origin',(0.,0.,0.));
#10846=CARTESIAN_POINT('',(0.,0.,0.));
#10847=CARTESIAN_POINT('Origin',(0.0721687836487032,0.,-0.125));
#10848=CARTESIAN_POINT('',(0.0721687836487032,0.,-0.125));
#10849=CARTESIAN_POINT('',(0.144337567297406,0.,0.));
#10850=CARTESIAN_POINT('',(0.117710979560879,0.,-0.0461186027918559));
#10851=CARTESIAN_POINT('',(0.0721687836487032,-0.25,-0.125));
#10852=CARTESIAN_POINT('',(0.0721687836487032,0.,-0.125));
#10853=CARTESIAN_POINT('',(0.144337567297406,-0.25,0.));
#10854=CARTESIAN_POINT('',(0.144337567297406,-0.25,0.));
#10855=CARTESIAN_POINT('',(0.144337567297406,0.,0.));
#10856=CARTESIAN_POINT('Origin',(-0.0721687836487032,0.,-0.125));
#10857=CARTESIAN_POINT('',(-0.0721687836487032,0.,-0.125));
#10858=CARTESIAN_POINT('',(0.0739156081756484,0.,-0.125));
#10859=CARTESIAN_POINT('',(-0.0721687836487032,-0.25,-0.125));
#10860=CARTESIAN_POINT('',(-0.0721687836487032,0.,-0.125));
#10861=CARTESIAN_POINT('',(0.0721687836487032,-0.25,-0.125));
#10862=CARTESIAN_POINT('Origin',(-0.144337567297406,0.,-4.16333634234434E-17));
#10863=CARTESIAN_POINT('',(-0.144337567297406,0.,-1.76762539787485E-17));
#10864=CARTESIAN_POINT('',(-0.0987953713852306,0.,-0.0788813972081442));
#10865=CARTESIAN_POINT('',(-0.144337567297406,-0.25,-2.77555756156289E-17));
#10866=CARTESIAN_POINT('',(-0.144337567297406,0.,-1.76762539787485E-17));
#10867=CARTESIAN_POINT('',(-0.0721687836487032,-0.25,-0.125));
#10868=CARTESIAN_POINT('Origin',(-0.0721687836487033,0.,0.125));
#10869=CARTESIAN_POINT('',(-0.0721687836487033,0.,0.125));
#10870=CARTESIAN_POINT('',(-0.0627109795608791,0.,0.141381397208144));
#10871=CARTESIAN_POINT('',(-0.0721687836487033,-0.25,0.125));
#10872=CARTESIAN_POINT('',(-0.0721687836487033,0.,0.125));
#10873=CARTESIAN_POINT('',(-0.144337567297406,-0.25,-1.76762539787485E-17));
#10874=CARTESIAN_POINT('Origin',(0.0721687836487032,0.,0.125));
#10875=CARTESIAN_POINT('',(0.0721687836487032,0.,0.125));
#10876=CARTESIAN_POINT('',(0.146084391824352,0.,0.125));
#10877=CARTESIAN_POINT('',(0.0721687836487032,-0.25,0.125));
#10878=CARTESIAN_POINT('',(0.0721687836487032,0.,0.125));
#10879=CARTESIAN_POINT('',(-0.0721687836487033,-0.25,0.125));
#10880=CARTESIAN_POINT('Origin',(0.144337567297406,0.,0.));
#10881=CARTESIAN_POINT('',(0.153795371385231,0.,-0.0163813972081441));
#10882=CARTESIAN_POINT('',(0.0721687836487032,-0.25,0.125));
#10883=CARTESIAN_POINT('Origin',(0.,-0.25,0.));
#10884=CARTESIAN_POINT('Origin',(0.22,0.,0.));
#10885=CARTESIAN_POINT('',(-0.22,-8.67361737988404E-18,-2.69422295812418E-17));
#10886=CARTESIAN_POINT('Origin',(0.,0.,0.));
#10887=CARTESIAN_POINT('Origin',(0.,-0.015,0.));
#10888=CARTESIAN_POINT('',(-0.24505,-0.02505,-3.00099698131059E-17));
#10889=CARTESIAN_POINT('Origin',(0.,-0.02505,0.));
#10890=CARTESIAN_POINT('',(-0.235,-0.015,-2.87791997799628E-17));
#10891=CARTESIAN_POINT('Origin',(0.,-0.3775,0.));
#10892=CARTESIAN_POINT('',(-0.24505,-0.72995,3.00099698131059E-17));
#10893=CARTESIAN_POINT('Origin',(0.,-0.72995,0.));
#10894=CARTESIAN_POINT('',(-0.24505,-0.3775,-3.00099698131059E-17));
#10895=CARTESIAN_POINT('Origin',(0.,-0.7625,0.));
#10896=CARTESIAN_POINT('',(-0.175,-0.8,-2.14313189850787E-17));
#10897=CARTESIAN_POINT('Origin',(0.,-0.8,0.));
#10898=CARTESIAN_POINT('',(-0.2125,-0.7625,-2.60237444818813E-17));
#10899=CARTESIAN_POINT('Origin',(0.,-0.8,0.));
#10900=CARTESIAN_POINT('',(0.,0.,0.));
#10901=CARTESIAN_POINT('',(0.,0.,0.));
#10902=CARTESIAN_POINT('',(0.,0.,0.));
#10903=CARTESIAN_POINT('',(0.,0.,0.));
#10904=CARTESIAN_POINT('',(0.,6.8,6.3));
#10905=CARTESIAN_POINT('',(0.,8.9,4.5));
#10906=CARTESIAN_POINT('',(0.,8.875,4.15));
#10907=CARTESIAN_POINT('',(0.,10.15,5.9));
#10908=CARTESIAN_POINT('',(0.,0.,0.));
#10909=CARTESIAN_POINT('',(0.,0.,0.));
#10910=UNCERTAINTY_MEASURE_WITH_UNIT(LENGTH_MEASURE(0.001),#10964,
'DISTANCE_ACCURACY_VALUE',
'Maximum model space distance between geometric entities at asserted c
onnectivities');
#10911=UNCERTAINTY_MEASURE_WITH_UNIT(LENGTH_MEASURE(0.001),#10964,
'DISTANCE_ACCURACY_VALUE',
'Maximum model space distance between geometric entities at asserted c
onnectivities');
#10912=UNCERTAINTY_MEASURE_WITH_UNIT(LENGTH_MEASURE(0.001),#10964,
'DISTANCE_ACCURACY_VALUE',
'Maximum model space distance between geometric entities at asserted c
onnectivities');
#10913=UNCERTAINTY_MEASURE_WITH_UNIT(LENGTH_MEASURE(0.001),#10964,
'DISTANCE_ACCURACY_VALUE',
'Maximum model space distance between geometric entities at asserted c
onnectivities');
#10914=UNCERTAINTY_MEASURE_WITH_UNIT(LENGTH_MEASURE(0.001),#10964,
'DISTANCE_ACCURACY_VALUE',
'Maximum model space distance between geometric entities at asserted c
onnectivities');
#10915=UNCERTAINTY_MEASURE_WITH_UNIT(LENGTH_MEASURE(0.001),#10964,
'DISTANCE_ACCURACY_VALUE',
'Maximum model space distance between geometric entities at asserted c
onnectivities');
#10916=UNCERTAINTY_MEASURE_WITH_UNIT(LENGTH_MEASURE(0.001),#10964,
'DISTANCE_ACCURACY_VALUE',
'Maximum model space distance between geometric entities at asserted c
onnectivities');
#10917=UNCERTAINTY_MEASURE_WITH_UNIT(LENGTH_MEASURE(0.001),#10964,
'DISTANCE_ACCURACY_VALUE',
'Maximum model space distance between geometric entities at asserted c
onnectivities');
#10918=UNCERTAINTY_MEASURE_WITH_UNIT(LENGTH_MEASURE(0.001),#10964,
'DISTANCE_ACCURACY_VALUE',
'Maximum model space distance between geometric entities at asserted c
onnectivities');
#10919=UNCERTAINTY_MEASURE_WITH_UNIT(LENGTH_MEASURE(0.001),#10964,
'DISTANCE_ACCURACY_VALUE',
'Maximum model space distance between geometric entities at asserted c
onnectivities');
#10920=UNCERTAINTY_MEASURE_WITH_UNIT(LENGTH_MEASURE(0.001),#10964,
'DISTANCE_ACCURACY_VALUE',
'Maximum model space distance between geometric entities at asserted c
onnectivities');
#10921=UNCERTAINTY_MEASURE_WITH_UNIT(LENGTH_MEASURE(0.001),#10964,
'DISTANCE_ACCURACY_VALUE',
'Maximum model space distance between geometric entities at asserted c
onnectivities');
#10922=UNCERTAINTY_MEASURE_WITH_UNIT(LENGTH_MEASURE(0.001),#10964,
'DISTANCE_ACCURACY_VALUE',
'Maximum model space distance between geometric entities at asserted c
onnectivities');
#10923=UNCERTAINTY_MEASURE_WITH_UNIT(LENGTH_MEASURE(0.001),#10964,
'DISTANCE_ACCURACY_VALUE',
'Maximum model space distance between geometric entities at asserted c
onnectivities');
#10924=UNCERTAINTY_MEASURE_WITH_UNIT(LENGTH_MEASURE(0.001),#10964,
'DISTANCE_ACCURACY_VALUE',
'Maximum model space distance between geometric entities at asserted c
onnectivities');
#10925=UNCERTAINTY_MEASURE_WITH_UNIT(LENGTH_MEASURE(0.001),#10964,
'DISTANCE_ACCURACY_VALUE',
'Maximum model space distance between geometric entities at asserted c
onnectivities');
#10926=UNCERTAINTY_MEASURE_WITH_UNIT(LENGTH_MEASURE(0.001),#10964,
'DISTANCE_ACCURACY_VALUE',
'Maximum model space distance between geometric entities at asserted c
onnectivities');
#10927=UNCERTAINTY_MEASURE_WITH_UNIT(LENGTH_MEASURE(0.001),#10964,
'DISTANCE_ACCURACY_VALUE',
'Maximum model space distance between geometric entities at asserted c
onnectivities');
#10928=UNCERTAINTY_MEASURE_WITH_UNIT(LENGTH_MEASURE(0.001),#10964,
'DISTANCE_ACCURACY_VALUE',
'Maximum model space distance between geometric entities at asserted c
onnectivities');
#10929=UNCERTAINTY_MEASURE_WITH_UNIT(LENGTH_MEASURE(0.001),#10964,
'DISTANCE_ACCURACY_VALUE',
'Maximum model space distance between geometric entities at asserted c
onnectivities');
#10930=UNCERTAINTY_MEASURE_WITH_UNIT(LENGTH_MEASURE(0.001),#10964,
'DISTANCE_ACCURACY_VALUE',
'Maximum model space distance between geometric entities at asserted c
onnectivities');
#10931=UNCERTAINTY_MEASURE_WITH_UNIT(LENGTH_MEASURE(0.001),#10964,
'DISTANCE_ACCURACY_VALUE',
'Maximum model space distance between geometric entities at asserted c
onnectivities');
#10932=UNCERTAINTY_MEASURE_WITH_UNIT(LENGTH_MEASURE(0.001),#10964,
'DISTANCE_ACCURACY_VALUE',
'Maximum model space distance between geometric entities at asserted c
onnectivities');
#10933=UNCERTAINTY_MEASURE_WITH_UNIT(LENGTH_MEASURE(0.001),#10964,
'DISTANCE_ACCURACY_VALUE',
'Maximum model space distance between geometric entities at asserted c
onnectivities');
#10934=UNCERTAINTY_MEASURE_WITH_UNIT(LENGTH_MEASURE(0.001),#10964,
'DISTANCE_ACCURACY_VALUE',
'Maximum model space distance between geometric entities at asserted c
onnectivities');
#10935=UNCERTAINTY_MEASURE_WITH_UNIT(LENGTH_MEASURE(0.001),#10964,
'DISTANCE_ACCURACY_VALUE',
'Maximum model space distance between geometric entities at asserted c
onnectivities');
#10936=UNCERTAINTY_MEASURE_WITH_UNIT(LENGTH_MEASURE(0.001),#10964,
'DISTANCE_ACCURACY_VALUE',
'Maximum model space distance between geometric entities at asserted c
onnectivities');
#10937=(
GEOMETRIC_REPRESENTATION_CONTEXT(3)
GLOBAL_UNCERTAINTY_ASSIGNED_CONTEXT((#10910))
GLOBAL_UNIT_ASSIGNED_CONTEXT((#10964,#10966,#10967))
REPRESENTATION_CONTEXT('','3D')
);
#10938=(
GEOMETRIC_REPRESENTATION_CONTEXT(3)
GLOBAL_UNCERTAINTY_ASSIGNED_CONTEXT((#10911))
GLOBAL_UNIT_ASSIGNED_CONTEXT((#10964,#10966,#10967))
REPRESENTATION_CONTEXT('','3D')
);
#10939=(
GEOMETRIC_REPRESENTATION_CONTEXT(3)
GLOBAL_UNCERTAINTY_ASSIGNED_CONTEXT((#10912))
GLOBAL_UNIT_ASSIGNED_CONTEXT((#10964,#10966,#10967))
REPRESENTATION_CONTEXT('','3D')
);
#10940=(
GEOMETRIC_REPRESENTATION_CONTEXT(3)
GLOBAL_UNCERTAINTY_ASSIGNED_CONTEXT((#10913))
GLOBAL_UNIT_ASSIGNED_CONTEXT((#10964,#10966,#10967))
REPRESENTATION_CONTEXT('','3D')
);
#10941=(
GEOMETRIC_REPRESENTATION_CONTEXT(3)
GLOBAL_UNCERTAINTY_ASSIGNED_CONTEXT((#10914))
GLOBAL_UNIT_ASSIGNED_CONTEXT((#10964,#10966,#10967))
REPRESENTATION_CONTEXT('','3D')
);
#10942=(
GEOMETRIC_REPRESENTATION_CONTEXT(3)
GLOBAL_UNCERTAINTY_ASSIGNED_CONTEXT((#10915))
GLOBAL_UNIT_ASSIGNED_CONTEXT((#10964,#10966,#10967))
REPRESENTATION_CONTEXT('','3D')
);
#10943=(
GEOMETRIC_REPRESENTATION_CONTEXT(3)
GLOBAL_UNCERTAINTY_ASSIGNED_CONTEXT((#10916))
GLOBAL_UNIT_ASSIGNED_CONTEXT((#10964,#10966,#10967))
REPRESENTATION_CONTEXT('','3D')
);
#10944=(
GEOMETRIC_REPRESENTATION_CONTEXT(3)
GLOBAL_UNCERTAINTY_ASSIGNED_CONTEXT((#10917))
GLOBAL_UNIT_ASSIGNED_CONTEXT((#10964,#10966,#10967))
REPRESENTATION_CONTEXT('','3D')
);
#10945=(
GEOMETRIC_REPRESENTATION_CONTEXT(3)
GLOBAL_UNCERTAINTY_ASSIGNED_CONTEXT((#10918))
GLOBAL_UNIT_ASSIGNED_CONTEXT((#10964,#10966,#10967))
REPRESENTATION_CONTEXT('','3D')
);
#10946=(
GEOMETRIC_REPRESENTATION_CONTEXT(3)
GLOBAL_UNCERTAINTY_ASSIGNED_CONTEXT((#10919))
GLOBAL_UNIT_ASSIGNED_CONTEXT((#10964,#10966,#10967))
REPRESENTATION_CONTEXT('','3D')
);
#10947=(
GEOMETRIC_REPRESENTATION_CONTEXT(3)
GLOBAL_UNCERTAINTY_ASSIGNED_CONTEXT((#10920))
GLOBAL_UNIT_ASSIGNED_CONTEXT((#10964,#10966,#10967))
REPRESENTATION_CONTEXT('','3D')
);
#10948=(
GEOMETRIC_REPRESENTATION_CONTEXT(3)
GLOBAL_UNCERTAINTY_ASSIGNED_CONTEXT((#10921))
GLOBAL_UNIT_ASSIGNED_CONTEXT((#10964,#10966,#10967))
REPRESENTATION_CONTEXT('','3D')
);
#10949=(
GEOMETRIC_REPRESENTATION_CONTEXT(3)
GLOBAL_UNCERTAINTY_ASSIGNED_CONTEXT((#10922))
GLOBAL_UNIT_ASSIGNED_CONTEXT((#10964,#10966,#10967))
REPRESENTATION_CONTEXT('','3D')
);
#10950=(
GEOMETRIC_REPRESENTATION_CONTEXT(3)
GLOBAL_UNCERTAINTY_ASSIGNED_CONTEXT((#10923))
GLOBAL_UNIT_ASSIGNED_CONTEXT((#10964,#10966,#10967))
REPRESENTATION_CONTEXT('','3D')
);
#10951=(
GEOMETRIC_REPRESENTATION_CONTEXT(3)
GLOBAL_UNCERTAINTY_ASSIGNED_CONTEXT((#10924))
GLOBAL_UNIT_ASSIGNED_CONTEXT((#10964,#10966,#10967))
REPRESENTATION_CONTEXT('','3D')
);
#10952=(
GEOMETRIC_REPRESENTATION_CONTEXT(3)
GLOBAL_UNCERTAINTY_ASSIGNED_CONTEXT((#10925))
GLOBAL_UNIT_ASSIGNED_CONTEXT((#10964,#10966,#10967))
REPRESENTATION_CONTEXT('','3D')
);
#10953=(
GEOMETRIC_REPRESENTATION_CONTEXT(3)
GLOBAL_UNCERTAINTY_ASSIGNED_CONTEXT((#10926))
GLOBAL_UNIT_ASSIGNED_CONTEXT((#10964,#10966,#10967))
REPRESENTATION_CONTEXT('','3D')
);
#10954=(
GEOMETRIC_REPRESENTATION_CONTEXT(3)
GLOBAL_UNCERTAINTY_ASSIGNED_CONTEXT((#10927))
GLOBAL_UNIT_ASSIGNED_CONTEXT((#10964,#10966,#10967))
REPRESENTATION_CONTEXT('','3D')
);
#10955=(
GEOMETRIC_REPRESENTATION_CONTEXT(3)
GLOBAL_UNCERTAINTY_ASSIGNED_CONTEXT((#10928))
GLOBAL_UNIT_ASSIGNED_CONTEXT((#10964,#10966,#10967))
REPRESENTATION_CONTEXT('','3D')
);
#10956=(
GEOMETRIC_REPRESENTATION_CONTEXT(3)
GLOBAL_UNCERTAINTY_ASSIGNED_CONTEXT((#10929))
GLOBAL_UNIT_ASSIGNED_CONTEXT((#10964,#10966,#10967))
REPRESENTATION_CONTEXT('','3D')
);
#10957=(
GEOMETRIC_REPRESENTATION_CONTEXT(3)
GLOBAL_UNCERTAINTY_ASSIGNED_CONTEXT((#10930))
GLOBAL_UNIT_ASSIGNED_CONTEXT((#10964,#10966,#10967))
REPRESENTATION_CONTEXT('','3D')
);
#10958=(
GEOMETRIC_REPRESENTATION_CONTEXT(3)
GLOBAL_UNCERTAINTY_ASSIGNED_CONTEXT((#10931))
GLOBAL_UNIT_ASSIGNED_CONTEXT((#10964,#10966,#10967))
REPRESENTATION_CONTEXT('','3D')
);
#10959=(
GEOMETRIC_REPRESENTATION_CONTEXT(3)
GLOBAL_UNCERTAINTY_ASSIGNED_CONTEXT((#10932))
GLOBAL_UNIT_ASSIGNED_CONTEXT((#10964,#10966,#10967))
REPRESENTATION_CONTEXT('','3D')
);
#10960=(
GEOMETRIC_REPRESENTATION_CONTEXT(3)
GLOBAL_UNCERTAINTY_ASSIGNED_CONTEXT((#10933))
GLOBAL_UNIT_ASSIGNED_CONTEXT((#10964,#10966,#10967))
REPRESENTATION_CONTEXT('','3D')
);
#10961=(
GEOMETRIC_REPRESENTATION_CONTEXT(3)
GLOBAL_UNCERTAINTY_ASSIGNED_CONTEXT((#10934))
GLOBAL_UNIT_ASSIGNED_CONTEXT((#10964,#10966,#10967))
REPRESENTATION_CONTEXT('','3D')
);
#10962=(
GEOMETRIC_REPRESENTATION_CONTEXT(3)
GLOBAL_UNCERTAINTY_ASSIGNED_CONTEXT((#10935))
GLOBAL_UNIT_ASSIGNED_CONTEXT((#10964,#10966,#10967))
REPRESENTATION_CONTEXT('','3D')
);
#10963=(
GEOMETRIC_REPRESENTATION_CONTEXT(3)
GLOBAL_UNCERTAINTY_ASSIGNED_CONTEXT((#10936))
GLOBAL_UNIT_ASSIGNED_CONTEXT((#10964,#10966,#10967))
REPRESENTATION_CONTEXT('','3D')
);
#10964=(
LENGTH_UNIT()
NAMED_UNIT(*)
SI_UNIT(.CENTI.,.METRE.)
);
#10965=(
LENGTH_UNIT()
NAMED_UNIT(*)
SI_UNIT($,.METRE.)
);
#10966=(
NAMED_UNIT(*)
PLANE_ANGLE_UNIT()
SI_UNIT($,.RADIAN.)
);
#10967=(
NAMED_UNIT(*)
SI_UNIT($,.STERADIAN.)
SOLID_ANGLE_UNIT()
);
#10968=SHAPE_DEFINITION_REPRESENTATION(#10994,#11057);
#10969=SHAPE_DEFINITION_REPRESENTATION(#10995,#11058);
#10970=SHAPE_DEFINITION_REPRESENTATION(#10996,#11059);
#10971=SHAPE_DEFINITION_REPRESENTATION(#10997,#11060);
#10972=SHAPE_DEFINITION_REPRESENTATION(#10998,#11061);
#10973=SHAPE_DEFINITION_REPRESENTATION(#10999,#11062);
#10974=SHAPE_DEFINITION_REPRESENTATION(#11000,#11063);
#10975=SHAPE_DEFINITION_REPRESENTATION(#11001,#11064);
#10976=SHAPE_DEFINITION_REPRESENTATION(#11002,#11065);
#10977=SHAPE_DEFINITION_REPRESENTATION(#11003,#11066);
#10978=SHAPE_DEFINITION_REPRESENTATION(#11004,#11067);
#10979=SHAPE_DEFINITION_REPRESENTATION(#11005,#11068);
#10980=SHAPE_DEFINITION_REPRESENTATION(#11006,#11069);
#10981=SHAPE_DEFINITION_REPRESENTATION(#11007,#11070);
#10982=SHAPE_DEFINITION_REPRESENTATION(#11008,#11071);
#10983=SHAPE_DEFINITION_REPRESENTATION(#11009,#11072);
#10984=SHAPE_DEFINITION_REPRESENTATION(#11015,#11073);
#10985=SHAPE_DEFINITION_REPRESENTATION(#11016,#11074);
#10986=SHAPE_DEFINITION_REPRESENTATION(#11039,#11075);
#10987=SHAPE_DEFINITION_REPRESENTATION(#11040,#11076);
#10988=SHAPE_DEFINITION_REPRESENTATION(#11041,#11077);
#10989=SHAPE_DEFINITION_REPRESENTATION(#11042,#11078);
#10990=SHAPE_DEFINITION_REPRESENTATION(#11043,#11079);
#10991=SHAPE_DEFINITION_REPRESENTATION(#11044,#11080);
#10992=SHAPE_DEFINITION_REPRESENTATION(#11045,#11081);
#10993=SHAPE_DEFINITION_REPRESENTATION(#11046,#11082);
#10994=PRODUCT_DEFINITION_SHAPE('',$,#11084);
#10995=PRODUCT_DEFINITION_SHAPE('',$,#11085);
#10996=PRODUCT_DEFINITION_SHAPE('',$,#11086);
#10997=PRODUCT_DEFINITION_SHAPE('',$,#11087);
#10998=PRODUCT_DEFINITION_SHAPE('',$,#11088);
#10999=PRODUCT_DEFINITION_SHAPE('',$,#11089);
#11000=PRODUCT_DEFINITION_SHAPE('',$,#11090);
#11001=PRODUCT_DEFINITION_SHAPE('',$,#11091);
#11002=PRODUCT_DEFINITION_SHAPE('',$,#11092);
#11003=PRODUCT_DEFINITION_SHAPE('',$,#11093);
#11004=PRODUCT_DEFINITION_SHAPE('',$,#11094);
#11005=PRODUCT_DEFINITION_SHAPE('',$,#11095);
#11006=PRODUCT_DEFINITION_SHAPE('',$,#11096);
#11007=PRODUCT_DEFINITION_SHAPE('',$,#11097);
#11008=PRODUCT_DEFINITION_SHAPE('',$,#11098);
#11009=PRODUCT_DEFINITION_SHAPE('',$,#11099);
#11010=PRODUCT_DEFINITION_SHAPE($,$,#126);
#11011=PRODUCT_DEFINITION_SHAPE($,$,#127);
#11012=PRODUCT_DEFINITION_SHAPE($,$,#128);
#11013=PRODUCT_DEFINITION_SHAPE($,$,#129);
#11014=PRODUCT_DEFINITION_SHAPE($,$,#130);
#11015=PRODUCT_DEFINITION_SHAPE('',$,#11100);
#11016=PRODUCT_DEFINITION_SHAPE('',$,#11101);
#11017=PRODUCT_DEFINITION_SHAPE($,$,#131);
#11018=PRODUCT_DEFINITION_SHAPE($,$,#132);
#11019=PRODUCT_DEFINITION_SHAPE($,$,#133);
#11020=PRODUCT_DEFINITION_SHAPE($,$,#134);
#11021=PRODUCT_DEFINITION_SHAPE($,$,#135);
#11022=PRODUCT_DEFINITION_SHAPE($,$,#136);
#11023=PRODUCT_DEFINITION_SHAPE($,$,#137);
#11024=PRODUCT_DEFINITION_SHAPE($,$,#138);
#11025=PRODUCT_DEFINITION_SHAPE($,$,#139);
#11026=PRODUCT_DEFINITION_SHAPE($,$,#140);
#11027=PRODUCT_DEFINITION_SHAPE($,$,#141);
#11028=PRODUCT_DEFINITION_SHAPE($,$,#142);
#11029=PRODUCT_DEFINITION_SHAPE($,$,#143);
#11030=PRODUCT_DEFINITION_SHAPE($,$,#144);
#11031=PRODUCT_DEFINITION_SHAPE($,$,#145);
#11032=PRODUCT_DEFINITION_SHAPE($,$,#146);
#11033=PRODUCT_DEFINITION_SHAPE($,$,#147);
#11034=PRODUCT_DEFINITION_SHAPE($,$,#148);
#11035=PRODUCT_DEFINITION_SHAPE($,$,#149);
#11036=PRODUCT_DEFINITION_SHAPE($,$,#150);
#11037=PRODUCT_DEFINITION_SHAPE($,$,#151);
#11038=PRODUCT_DEFINITION_SHAPE($,$,#152);
#11039=PRODUCT_DEFINITION_SHAPE('',$,#11102);
#11040=PRODUCT_DEFINITION_SHAPE('',$,#11103);
#11041=PRODUCT_DEFINITION_SHAPE('',$,#11104);
#11042=PRODUCT_DEFINITION_SHAPE('',$,#11105);
#11043=PRODUCT_DEFINITION_SHAPE('',$,#11106);
#11044=PRODUCT_DEFINITION_SHAPE('',$,#11107);
#11045=PRODUCT_DEFINITION_SHAPE('',$,#11108);
#11046=PRODUCT_DEFINITION_SHAPE('',$,#11109);
#11047=PRODUCT_DEFINITION_SHAPE($,$,#153);
#11048=PRODUCT_DEFINITION_SHAPE($,$,#154);
#11049=PRODUCT_DEFINITION_SHAPE($,$,#155);
#11050=PRODUCT_DEFINITION_SHAPE($,$,#156);
#11051=PRODUCT_DEFINITION_SHAPE($,$,#157);
#11052=PRODUCT_DEFINITION_SHAPE($,$,#158);
#11053=PRODUCT_DEFINITION_SHAPE($,$,#159);
#11054=PRODUCT_DEFINITION_SHAPE($,$,#160);
#11055=PRODUCT_DEFINITION_SHAPE($,$,#161);
#11056=PRODUCT_DEFINITION_SHAPE($,$,#162);
#11057=SHAPE_REPRESENTATION('',(#5925,#6686,#6687),#10937);
#11058=SHAPE_REPRESENTATION('',(#5926,#6297,#6298,#6299,#6300,#6301,#6302,
#6303,#6304,#6305,#6306,#6307,#6308,#6309,#6310,#6311,#6312,#6313,#6314,
#6315,#6316,#6317,#6318),#10938);
#11059=SHAPE_REPRESENTATION('',(#5927),#10939);
#11060=SHAPE_REPRESENTATION('',(#5946),#10940);
#11061=SHAPE_REPRESENTATION('',(#6025),#10941);
#11062=SHAPE_REPRESENTATION('',(#6034),#10942);
#11063=SHAPE_REPRESENTATION('',(#6063),#10943);
#11064=SHAPE_REPRESENTATION('',(#6072),#10944);
#11065=SHAPE_REPRESENTATION('',(#6097),#10945);
#11066=SHAPE_REPRESENTATION('',(#6104),#10946);
#11067=SHAPE_REPRESENTATION('',(#6111,#6240,#6241,#6242,#6243,#6244),#10947);
#11068=SHAPE_REPRESENTATION('',(#6112),#10948);
#11069=SHAPE_REPRESENTATION('',(#6132),#10949);
#11070=SHAPE_REPRESENTATION('',(#6152),#10950);
#11071=SHAPE_REPRESENTATION('',(#6169),#10951);
#11072=SHAPE_REPRESENTATION('',(#6223),#10952);
#11073=SHAPE_REPRESENTATION('',(#6245),#10953);
#11074=SHAPE_REPRESENTATION('',(#6271),#10954);
#11075=SHAPE_REPRESENTATION('',(#6319,#6678,#6679,#6680,#6681,#6682,#6683,
#6684,#6685),#10955);
#11076=SHAPE_REPRESENTATION('',(#6320),#10956);
#11077=SHAPE_REPRESENTATION('',(#6345),#10957);
#11078=SHAPE_REPRESENTATION('',(#6354),#10958);
#11079=SHAPE_REPRESENTATION('',(#6369),#10959);
#11080=SHAPE_REPRESENTATION('',(#6384),#10960);
#11081=SHAPE_REPRESENTATION('',(#6650),#10961);
#11082=SHAPE_REPRESENTATION('',(#6661),#10962);
#11083=PRODUCT_DEFINITION_CONTEXT('part definition',#11163,'design');
#11084=PRODUCT_DEFINITION('PAT-076',
'PAT-076',#11110,#11083);
#11085=PRODUCT_DEFINITION('Bearing housing','Bearing housing',#11111,#11083);
#11086=PRODUCT_DEFINITION('Base','Base',#11112,#11083);
#11087=PRODUCT_DEFINITION('Housing','Housing',#11113,#11083);
#11088=PRODUCT_DEFINITION('Outer race spacer','Outer race spacer',#11114,
#11083);
#11089=PRODUCT_DEFINITION('Seal cap','Seal cap',#11115,#11083);
#11090=PRODUCT_DEFINITION('Dust seal envelope','Dust seal envelope',#11116,
#11083);
#11091=PRODUCT_DEFINITION('Rear cap','Rear cap',#11117,#11083);
#11092=PRODUCT_DEFINITION('Bonded base pad','Bonded base pad',#11118,#11083);
#11093=PRODUCT_DEFINITION('Bonded base pad (1)','Bonded base pad (1)',#11119,
#11083);
#11094=PRODUCT_DEFINITION('Sealed Ball Bearing - 20 x 47 x 14 mm',
'Sealed Ball Bearing - 20 x 47 x 14 mm',#11120,#11083);
#11095=PRODUCT_DEFINITION('Inner ring','Inner ring',#11121,#11083);
#11096=PRODUCT_DEFINITION('Outer ring','Outer ring',#11122,#11083);
#11097=PRODUCT_DEFINITION('Balls','Balls',#11123,#11083);
#11098=PRODUCT_DEFINITION('Cage','Cage',#11124,#11083);
#11099=PRODUCT_DEFINITION('Seals 2RS','Seals 2RS',#11125,#11083);
#11100=PRODUCT_DEFINITION('Cap Screw - M6x25','Cap Screw - M6x25',#11126,
#11083);
#11101=PRODUCT_DEFINITION('Cap Screw - M4x16','Cap Screw - M4x16',#11127,
#11083);
#11102=PRODUCT_DEFINITION('Shaft and drive','Shaft and drive',#11128,#11083);
#11103=PRODUCT_DEFINITION('Stepped shaft','Stepped shaft',#11129,#11083);
#11104=PRODUCT_DEFINITION('Inner race spacer','Inner race spacer',#11130,
#11083);
#11105=PRODUCT_DEFINITION('Shaft collar','Shaft collar',#11131,#11083);
#11106=PRODUCT_DEFINITION('Pulley collar','Pulley collar',#11132,#11083);
#11107=PRODUCT_DEFINITION(
'Timing Pulley - 2 mm Pitch, 40 Teeth, 12 mm Bore',
'Timing Pulley - 2 mm Pitch, 40 Teeth, 12 mm Bore',#11133,#11083);
#11108=PRODUCT_DEFINITION('Key 4x4x14','Key 4x4x14',#11134,#11083);
#11109=PRODUCT_DEFINITION('Socket Set Screw - M5x8',
'Socket Set Screw - M5x8',#11135,#11083);
#11110=PRODUCT_DEFINITION_FORMATION('',$,#11165);
#11111=PRODUCT_DEFINITION_FORMATION('',$,#11166);
#11112=PRODUCT_DEFINITION_FORMATION('',$,#11167);
#11113=PRODUCT_DEFINITION_FORMATION('',$,#11168);
#11114=PRODUCT_DEFINITION_FORMATION('',$,#11169);
#11115=PRODUCT_DEFINITION_FORMATION('',$,#11170);
#11116=PRODUCT_DEFINITION_FORMATION('',$,#11171);
#11117=PRODUCT_DEFINITION_FORMATION('',$,#11172);
#11118=PRODUCT_DEFINITION_FORMATION('',$,#11173);
#11119=PRODUCT_DEFINITION_FORMATION('',$,#11174);
#11120=PRODUCT_DEFINITION_FORMATION('',$,#11175);
#11121=PRODUCT_DEFINITION_FORMATION('',$,#11176);
#11122=PRODUCT_DEFINITION_FORMATION('',$,#11177);
#11123=PRODUCT_DEFINITION_FORMATION('',$,#11178);
#11124=PRODUCT_DEFINITION_FORMATION('',$,#11179);
#11125=PRODUCT_DEFINITION_FORMATION('',$,#11180);
#11126=PRODUCT_DEFINITION_FORMATION('',$,#11181);
#11127=PRODUCT_DEFINITION_FORMATION('',$,#11182);
#11128=PRODUCT_DEFINITION_FORMATION('',$,#11183);
#11129=PRODUCT_DEFINITION_FORMATION('',$,#11184);
#11130=PRODUCT_DEFINITION_FORMATION('',$,#11185);
#11131=PRODUCT_DEFINITION_FORMATION('',$,#11186);
#11132=PRODUCT_DEFINITION_FORMATION('',$,#11187);
#11133=PRODUCT_DEFINITION_FORMATION('',$,#11188);
#11134=PRODUCT_DEFINITION_FORMATION('',$,#11189);
#11135=PRODUCT_DEFINITION_FORMATION('',$,#11190);
#11136=PRODUCT_RELATED_PRODUCT_CATEGORY('PAT-076','PAT-076',(#11165));
#11137=PRODUCT_RELATED_PRODUCT_CATEGORY('Bearing housing',
'Bearing housing',(#11166));
#11138=PRODUCT_RELATED_PRODUCT_CATEGORY('Base','Base',(#11167));
#11139=PRODUCT_RELATED_PRODUCT_CATEGORY('Housing','Housing',(#11168));
#11140=PRODUCT_RELATED_PRODUCT_CATEGORY('Outer race spacer',
'Outer race spacer',(#11169));
#11141=PRODUCT_RELATED_PRODUCT_CATEGORY('Seal cap','Seal cap',(#11170));
#11142=PRODUCT_RELATED_PRODUCT_CATEGORY('Dust seal envelope',
'Dust seal envelope',(#11171));
#11143=PRODUCT_RELATED_PRODUCT_CATEGORY('Rear cap','Rear cap',(#11172));
#11144=PRODUCT_RELATED_PRODUCT_CATEGORY('Bonded base pad',
'Bonded base pad',(#11173));
#11145=PRODUCT_RELATED_PRODUCT_CATEGORY('Bonded base pad (1)',
'Bonded base pad (1)',(#11174));
#11146=PRODUCT_RELATED_PRODUCT_CATEGORY(
'Sealed Ball Bearing - 20 x 47 x 14 mm',
'Sealed Ball Bearing - 20 x 47 x 14 mm',(#11175));
#11147=PRODUCT_RELATED_PRODUCT_CATEGORY('Inner ring','Inner ring',(#11176));
#11148=PRODUCT_RELATED_PRODUCT_CATEGORY('Outer ring','Outer ring',(#11177));
#11149=PRODUCT_RELATED_PRODUCT_CATEGORY('Balls','Balls',(#11178));
#11150=PRODUCT_RELATED_PRODUCT_CATEGORY('Cage','Cage',(#11179));
#11151=PRODUCT_RELATED_PRODUCT_CATEGORY('Seals 2RS','Seals 2RS',(#11180));
#11152=PRODUCT_RELATED_PRODUCT_CATEGORY('Cap Screw - M6x25',
'Cap Screw - M6x25',(#11181));
#11153=PRODUCT_RELATED_PRODUCT_CATEGORY('Cap Screw - M4x16',
'Cap Screw - M4x16',(#11182));
#11154=PRODUCT_RELATED_PRODUCT_CATEGORY('Shaft and drive',
'Shaft and drive',(#11183));
#11155=PRODUCT_RELATED_PRODUCT_CATEGORY('Stepped shaft','Stepped shaft',
(#11184));
#11156=PRODUCT_RELATED_PRODUCT_CATEGORY('Inner race spacer',
'Inner race spacer',(#11185));
#11157=PRODUCT_RELATED_PRODUCT_CATEGORY('Shaft collar','Shaft collar',(#11186));
#11158=PRODUCT_RELATED_PRODUCT_CATEGORY('Pulley collar','Pulley collar',
(#11187));
#11159=PRODUCT_RELATED_PRODUCT_CATEGORY(
'Timing Pulley - 2 mm Pitch, 40 Teeth, 12 mm Bore',
'Timing Pulley - 2 mm Pitch, 40 Teeth, 12 mm Bore',(#11188));
#11160=PRODUCT_RELATED_PRODUCT_CATEGORY('Key 4x4x14','Key 4x4x14',(#11189));
#11161=PRODUCT_RELATED_PRODUCT_CATEGORY('Socket Set Screw - M5x8',
'Socket Set Screw - M5x8',(#11190));
#11162=APPLICATION_PROTOCOL_DEFINITION('international standard',
'automotive_design',2009,#11163);
#11163=APPLICATION_CONTEXT(
'Core Data for Automotive Mechanical Design Process');
#11164=PRODUCT_CONTEXT('part definition',#11163,'mechanical');
#11165=PRODUCT('PAT-076','PAT-076',
'PAT-076',(#11164));
#11166=PRODUCT('Bearing housing','Bearing housing','Bearing housing',(#11164));
#11167=PRODUCT('Base','Base','Base',(#11164));
#11168=PRODUCT('Housing','Housing','Housing',(#11164));
#11169=PRODUCT('Outer race spacer','Outer race spacer',
'Outer race spacer',(#11164));
#11170=PRODUCT('Seal cap','Seal cap','Seal cap',(#11164));
#11171=PRODUCT('Dust seal envelope','Dust seal envelope',
'Dust seal envelope',(#11164));
#11172=PRODUCT('Rear cap','Rear cap','Rear cap',(#11164));
#11173=PRODUCT('Bonded base pad','Bonded base pad','Bonded base pad',(#11164));
#11174=PRODUCT('Bonded base pad (1)','Bonded base pad (1)',
'Bonded base pad (1)',(#11164));
#11175=PRODUCT('Sealed Ball Bearing - 20 x 47 x 14 mm',
'Sealed Ball Bearing - 20 x 47 x 14 mm',
'Sealed Ball Bearing - 20 x 47 x 14 mm',(#11164));
#11176=PRODUCT('Inner ring','Inner ring','Inner ring',(#11164));
#11177=PRODUCT('Outer ring','Outer ring','Outer ring',(#11164));
#11178=PRODUCT('Balls','Balls','Balls',(#11164));
#11179=PRODUCT('Cage','Cage','Cage',(#11164));
#11180=PRODUCT('Seals 2RS','Seals 2RS','Seals 2RS',(#11164));
#11181=PRODUCT('Cap Screw - M6x25','Cap Screw - M6x25',
'Cap Screw - M6x25',(#11164));
#11182=PRODUCT('Cap Screw - M4x16','Cap Screw - M4x16',
'Cap Screw - M4x16',(#11164));
#11183=PRODUCT('Shaft and drive','Shaft and drive','Shaft and drive',(#11164));
#11184=PRODUCT('Stepped shaft','Stepped shaft','Stepped shaft',(#11164));
#11185=PRODUCT('Inner race spacer','Inner race spacer',
'Inner race spacer',(#11164));
#11186=PRODUCT('Shaft collar','Shaft collar','Shaft collar',(#11164));
#11187=PRODUCT('Pulley collar','Pulley collar','Pulley collar',(#11164));
#11188=PRODUCT('Timing Pulley - 2 mm Pitch, 40 Teeth, 12 mm Bore',
'Timing Pulley - 2 mm Pitch, 40 Teeth, 12 mm Bore',
'Timing Pulley - 2 mm Pitch, 40 Teeth, 12 mm Bore',(#11164));
#11189=PRODUCT('Key 4x4x14','Key 4x4x14','Key 4x4x14',(#11164));
#11190=PRODUCT('Socket Set Screw - M5x8','Socket Set Screw - M5x8',
'Socket Set Screw - M5x8',(#11164));
#11191=PRESENTATION_STYLE_ASSIGNMENT((#11196));
#11192=PRESENTATION_STYLE_ASSIGNMENT((#11197));
#11193=PRESENTATION_STYLE_ASSIGNMENT((#11198));
#11194=PRESENTATION_STYLE_ASSIGNMENT((#11199));
#11195=PRESENTATION_STYLE_ASSIGNMENT((#11200));
#11196=SURFACE_STYLE_USAGE(.BOTH.,#11201);
#11197=SURFACE_STYLE_USAGE(.BOTH.,#11202);
#11198=SURFACE_STYLE_USAGE(.BOTH.,#11203);
#11199=SURFACE_STYLE_USAGE(.BOTH.,#11204);
#11200=SURFACE_STYLE_USAGE(.BOTH.,#11205);
#11201=SURFACE_SIDE_STYLE('',(#11206));
#11202=SURFACE_SIDE_STYLE('',(#11207));
#11203=SURFACE_SIDE_STYLE('',(#11208));
#11204=SURFACE_SIDE_STYLE('',(#11209));
#11205=SURFACE_SIDE_STYLE('',(#11210));
#11206=SURFACE_STYLE_FILL_AREA(#11211);
#11207=SURFACE_STYLE_FILL_AREA(#11212);
#11208=SURFACE_STYLE_FILL_AREA(#11213);
#11209=SURFACE_STYLE_FILL_AREA(#11214);
#11210=SURFACE_STYLE_FILL_AREA(#11215);
#11211=FILL_AREA_STYLE('Steel - Satin',(#11216));
#11212=FILL_AREA_STYLE('CAD Library Painted - Deep blue',(#11217));
#11213=FILL_AREA_STYLE('CAD Library Painted - Engineering blue',(#11218));
#11214=FILL_AREA_STYLE('CAD Library Painted - Steel gray',(#11219));
#11215=FILL_AREA_STYLE('CAD Library Painted - Graphite',(#11220));
#11216=FILL_AREA_STYLE_COLOUR('Steel - Satin',#11221);
#11217=FILL_AREA_STYLE_COLOUR('CAD Library Painted - Deep blue',#11222);
#11218=FILL_AREA_STYLE_COLOUR('CAD Library Painted - Engineering blue',
#11223);
#11219=FILL_AREA_STYLE_COLOUR('CAD Library Painted - Steel gray',#11224);
#11220=FILL_AREA_STYLE_COLOUR('CAD Library Painted - Graphite',#11225);
#11221=COLOUR_RGB('Steel - Satin',0.627450980392157,0.627450980392157,0.627450980392157);
#11222=COLOUR_RGB('CAD Library Painted - Deep blue',0.0784313725490196,
0.203921568627451,0.349019607843137);
#11223=COLOUR_RGB('CAD Library Painted - Engineering blue',0.12156862745098,
0.356862745098039,0.6);
#11224=COLOUR_RGB('CAD Library Painted - Steel gray',0.592156862745098,
0.631372549019608,0.67843137254902);
#11225=COLOUR_RGB('CAD Library Painted - Graphite',0.168627450980392,0.192156862745098,
0.231372549019608);
#11226=COLOUR_RGB('Dark Blue',0.08,0.2,0.34);
#11227=FILL_AREA_STYLE_COLOUR('',#11226);
#11228=FILL_AREA_STYLE('',(#11227));
#11229=SURFACE_STYLE_FILL_AREA(#11228);
#11230=SURFACE_SIDE_STYLE('',(#11229));
#11231=SURFACE_STYLE_USAGE(.BOTH.,#11230);
#11232=PRESENTATION_STYLE_ASSIGNMENT((#11231));
#11233=COLOUR_RGB('Light Blue',0.38,0.62,0.78);
#11234=FILL_AREA_STYLE_COLOUR('',#11233);
#11235=FILL_AREA_STYLE('',(#11234));
#11236=SURFACE_STYLE_FILL_AREA(#11235);
#11237=SURFACE_SIDE_STYLE('',(#11236));
#11238=SURFACE_STYLE_USAGE(.BOTH.,#11237);
#11239=PRESENTATION_STYLE_ASSIGNMENT((#11238));
#11240=COLOUR_RGB('Sky Blue',0.24,0.69,0.87);
#11241=FILL_AREA_STYLE_COLOUR('',#11240);
#11242=FILL_AREA_STYLE('',(#11241));
#11243=SURFACE_STYLE_FILL_AREA(#11242);
#11244=SURFACE_SIDE_STYLE('',(#11243));
#11245=SURFACE_STYLE_USAGE(.BOTH.,#11244);
#11246=PRESENTATION_STYLE_ASSIGNMENT((#11245));
#11247=COLOUR_RGB('Grey',0.48,0.52,0.57);
#11248=FILL_AREA_STYLE_COLOUR('',#11247);
#11249=FILL_AREA_STYLE('',(#11248));
#11250=SURFACE_STYLE_FILL_AREA(#11249);
#11251=SURFACE_SIDE_STYLE('',(#11250));
#11252=SURFACE_STYLE_USAGE(.BOTH.,#11251);
#11253=PRESENTATION_STYLE_ASSIGNMENT((#11252));
#11254=COLOUR_RGB('Black',0.12,0.14,0.17);
#11255=FILL_AREA_STYLE_COLOUR('',#11254);
#11256=FILL_AREA_STYLE('',(#11255));
#11257=SURFACE_STYLE_FILL_AREA(#11256);
#11258=SURFACE_SIDE_STYLE('',(#11257));
#11259=SURFACE_STYLE_USAGE(.BOTH.,#11258);
#11260=PRESENTATION_STYLE_ASSIGNMENT((#11259));
#11261=COLOUR_RGB('Off White',0.89,0.88,0.83);
#11262=FILL_AREA_STYLE_COLOUR('',#11261);
#11263=FILL_AREA_STYLE('',(#11262));
#11264=SURFACE_STYLE_FILL_AREA(#11263);
#11265=SURFACE_SIDE_STYLE('',(#11264));
#11266=SURFACE_STYLE_USAGE(.BOTH.,#11265);
#11267=PRESENTATION_STYLE_ASSIGNMENT((#11266));
ENDSEC;
END-ISO-10303-21;
